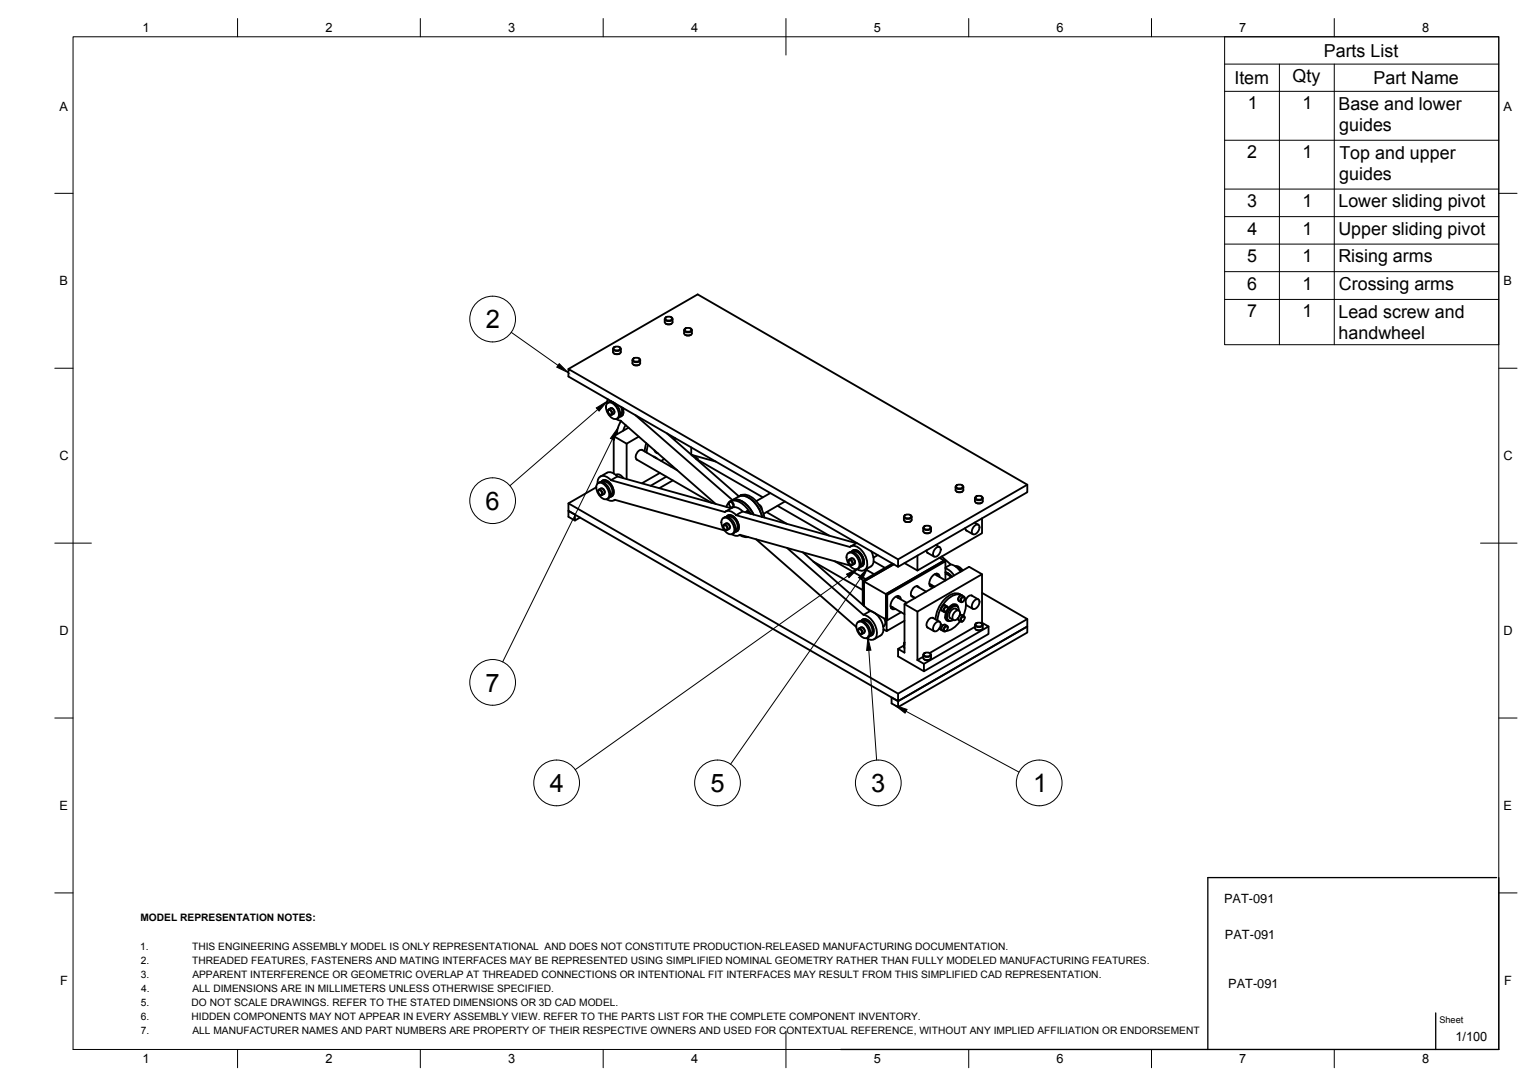
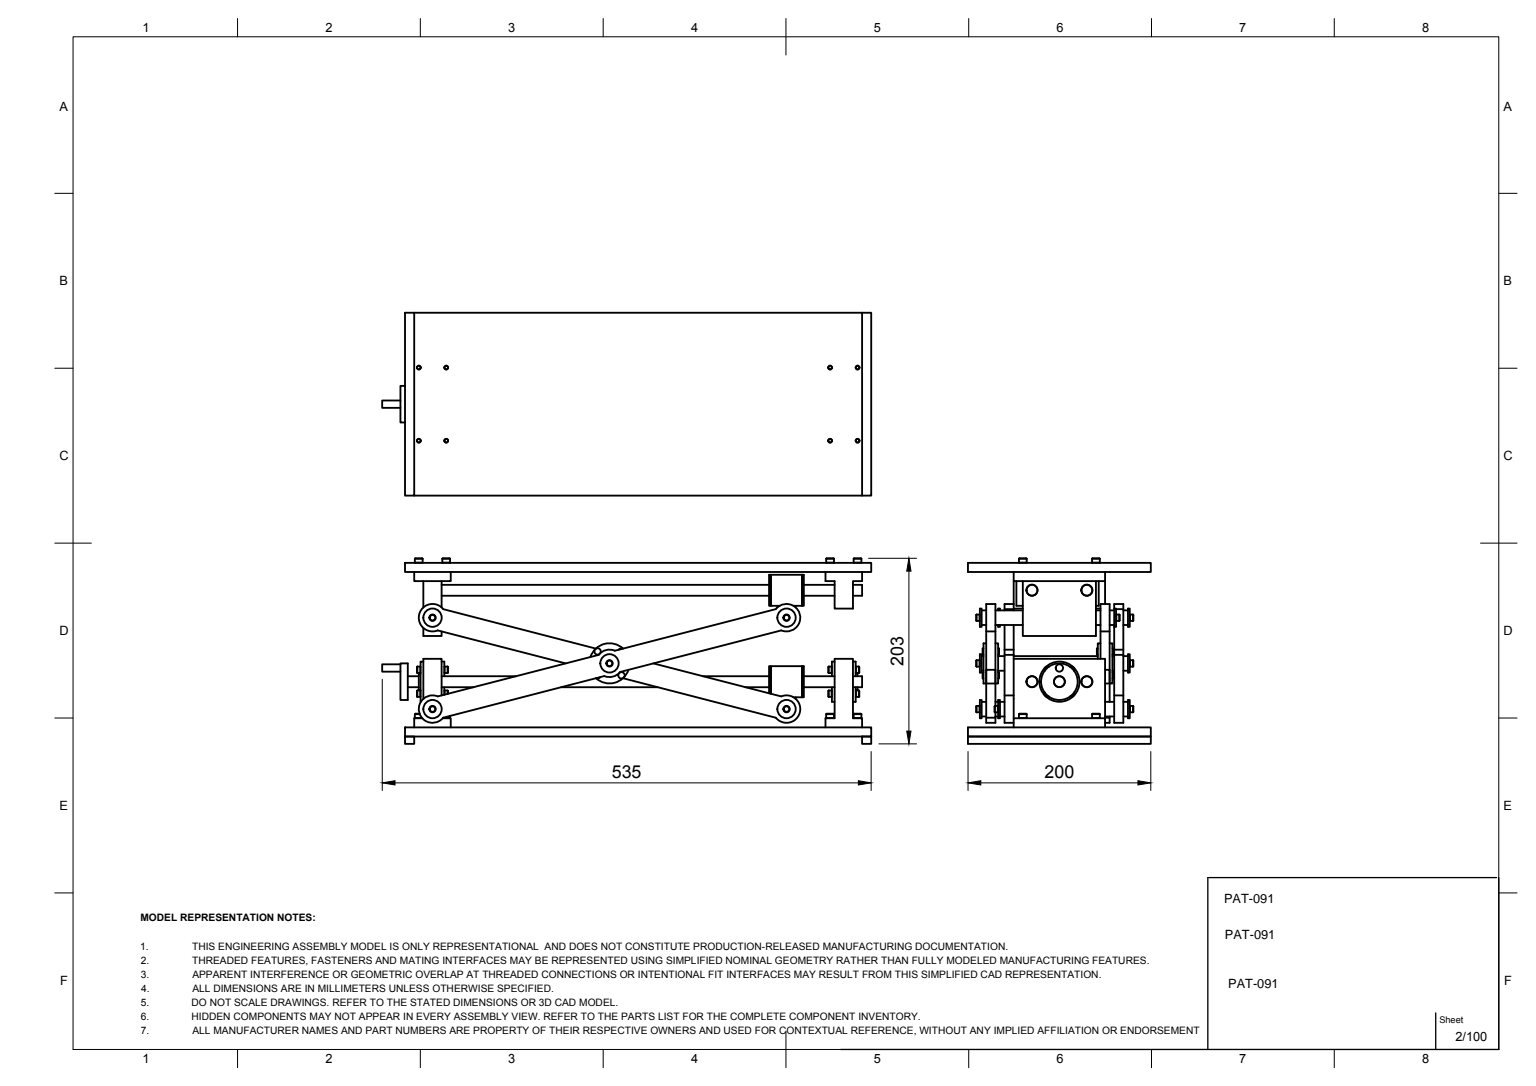
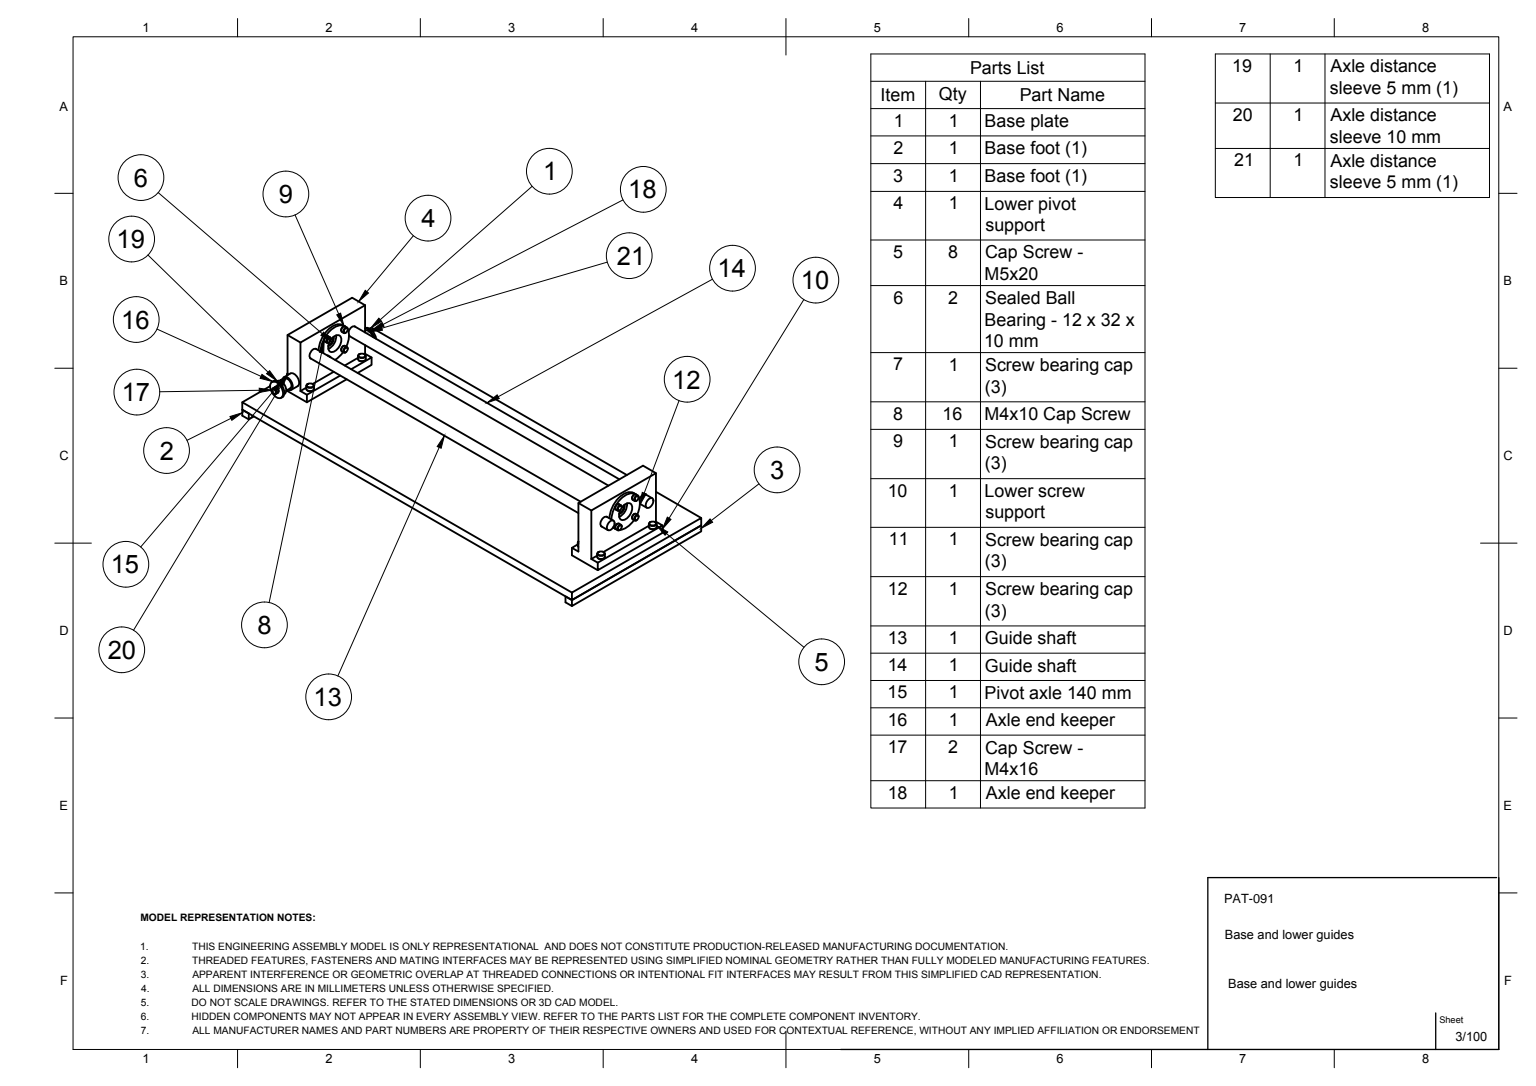
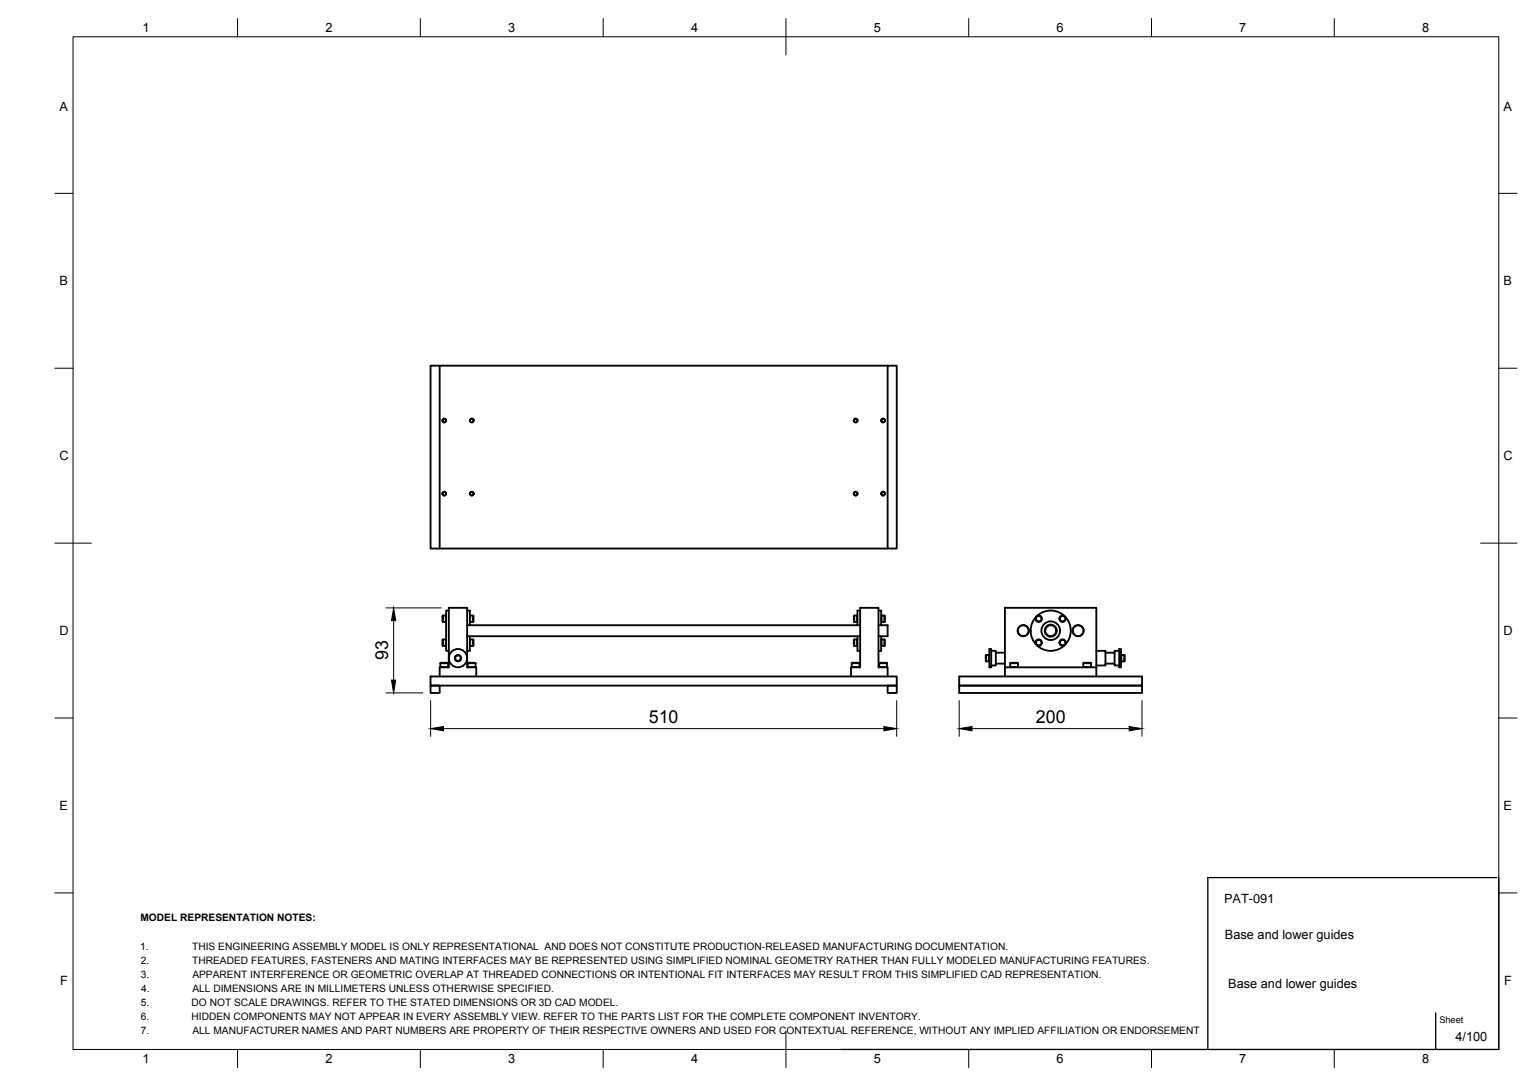
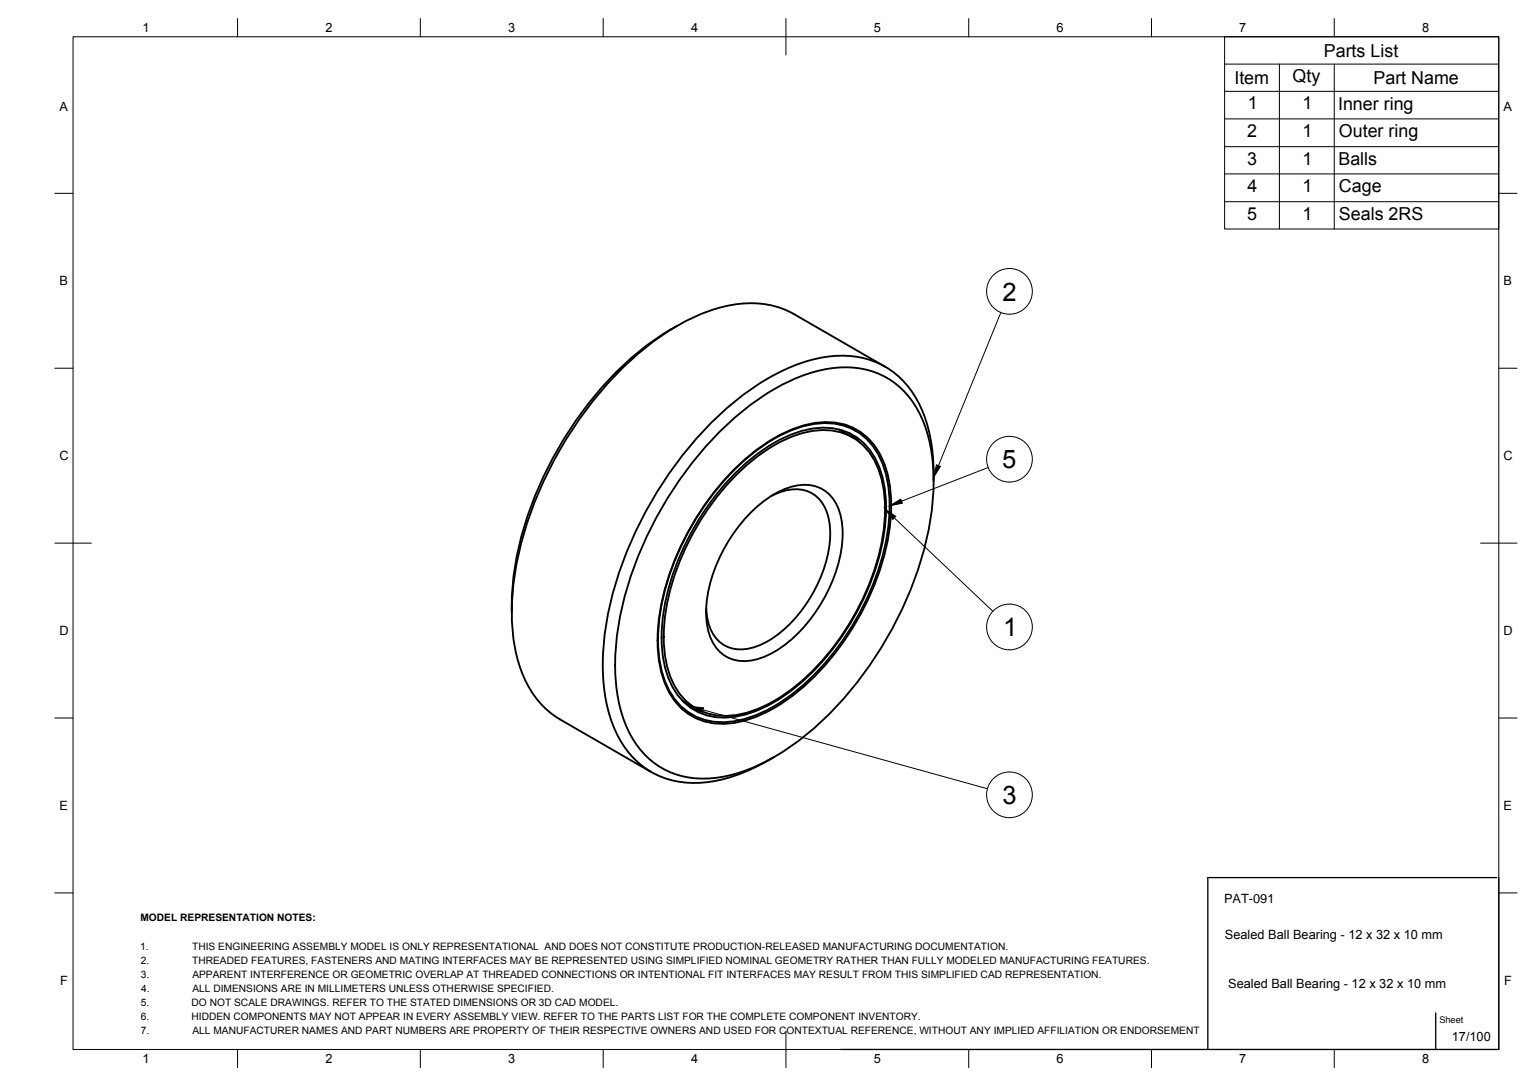
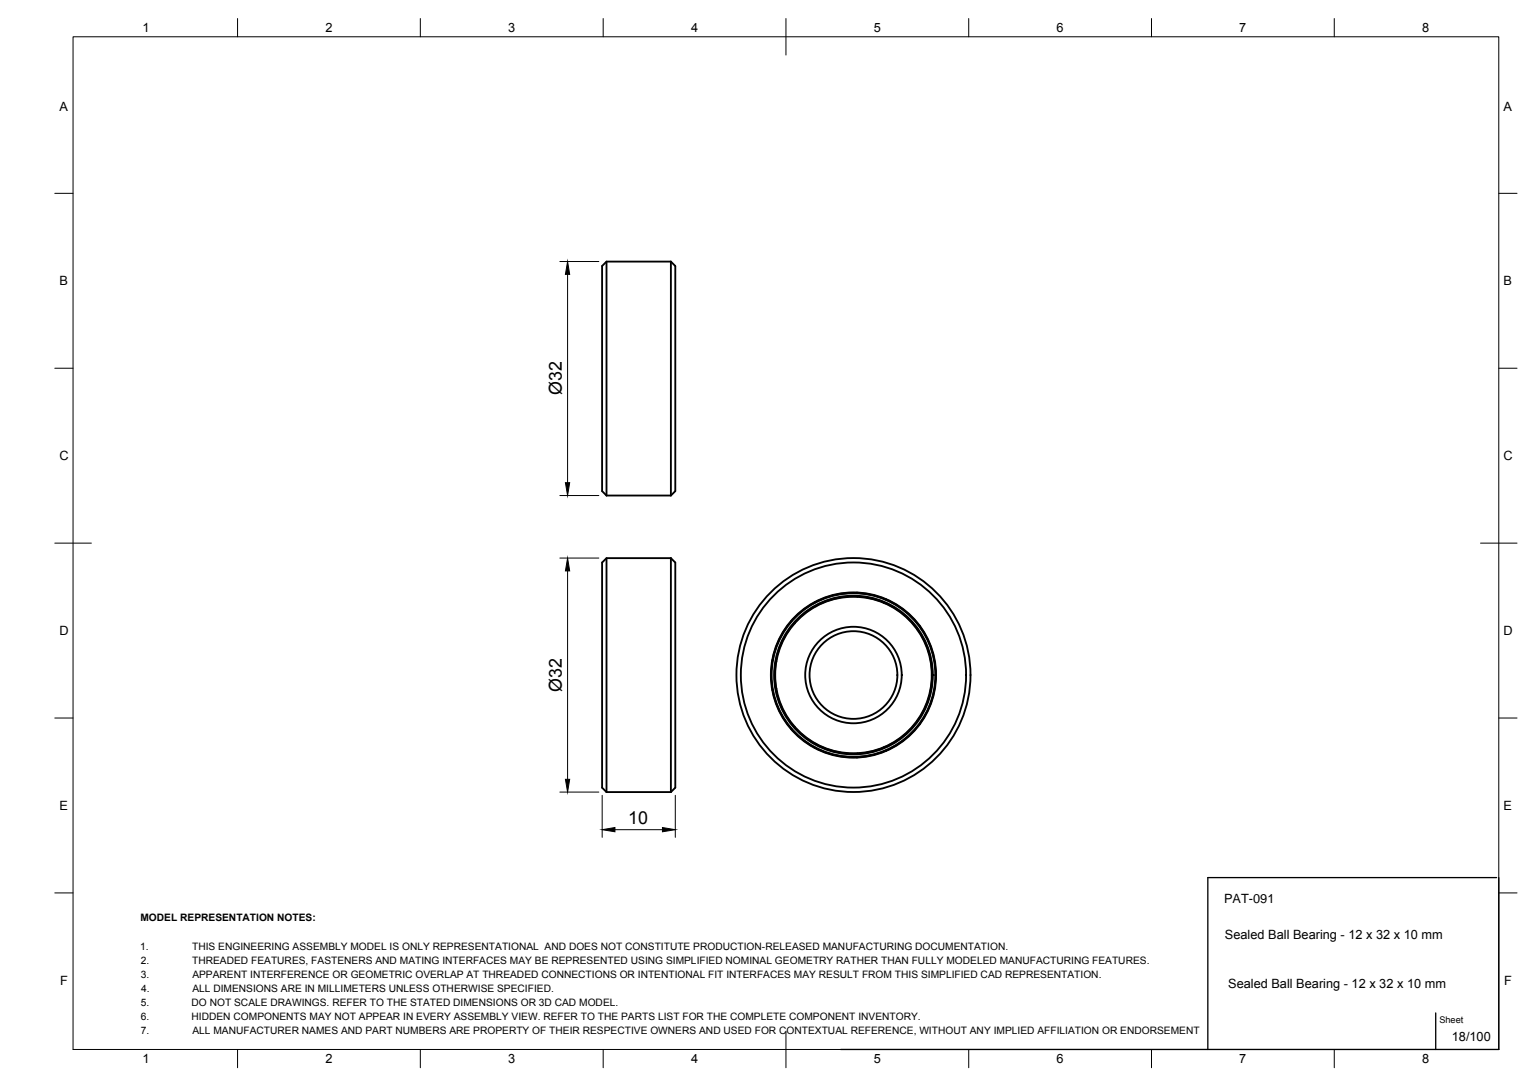
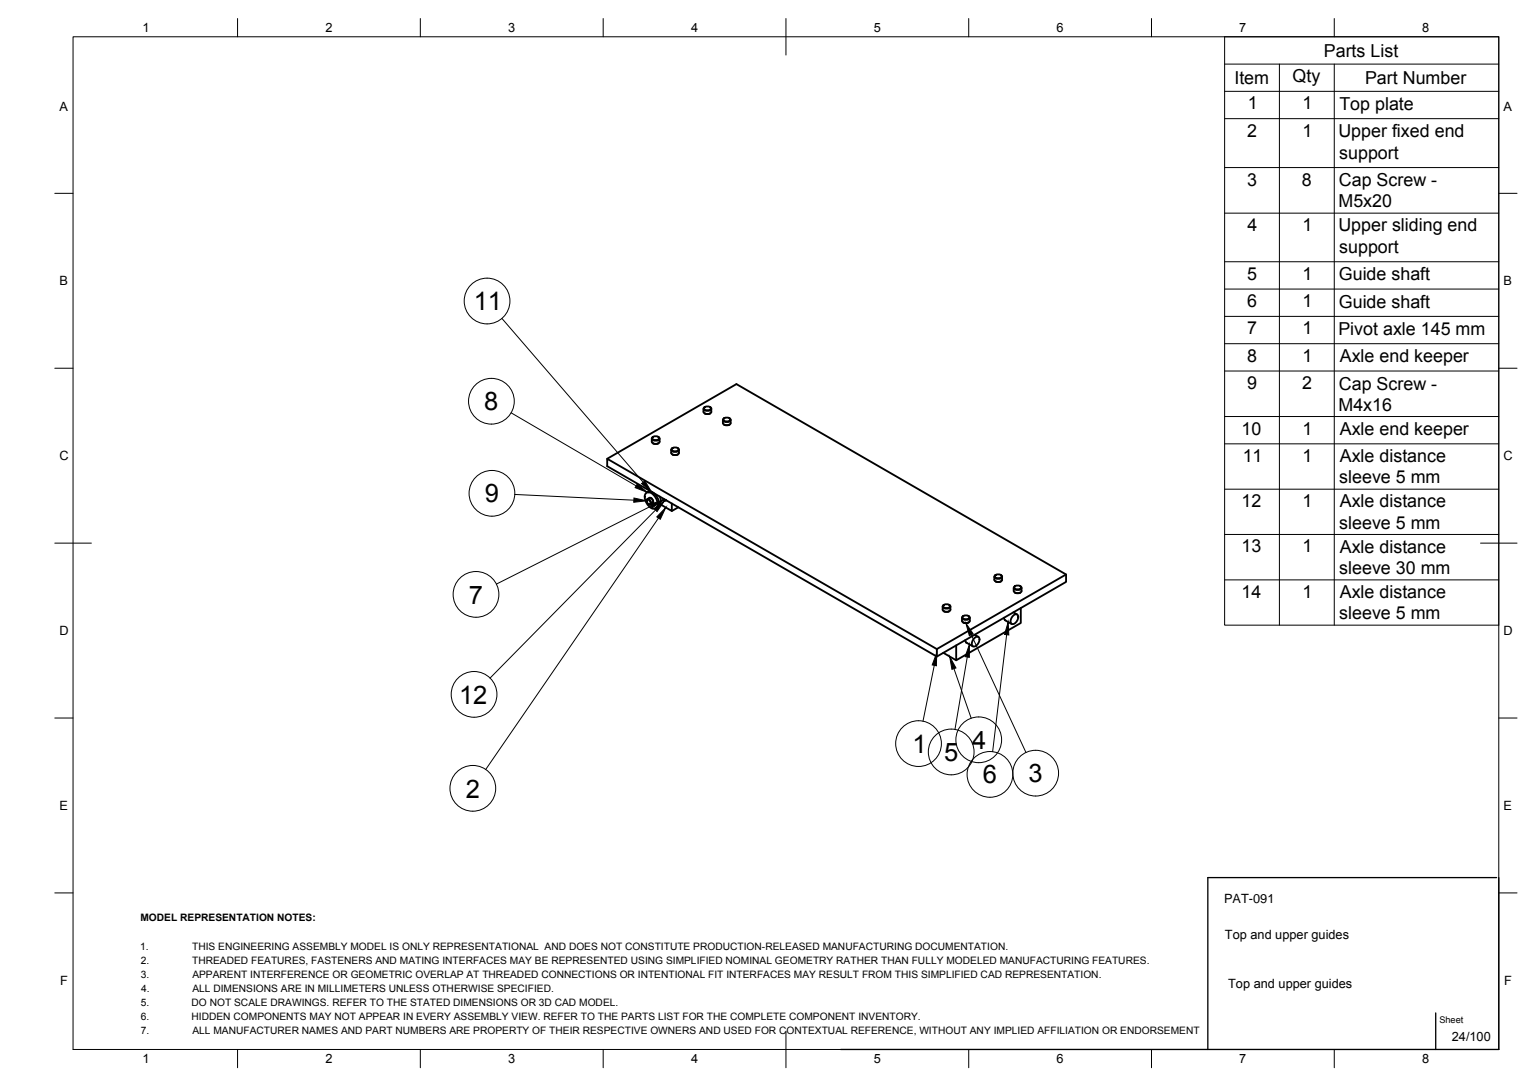
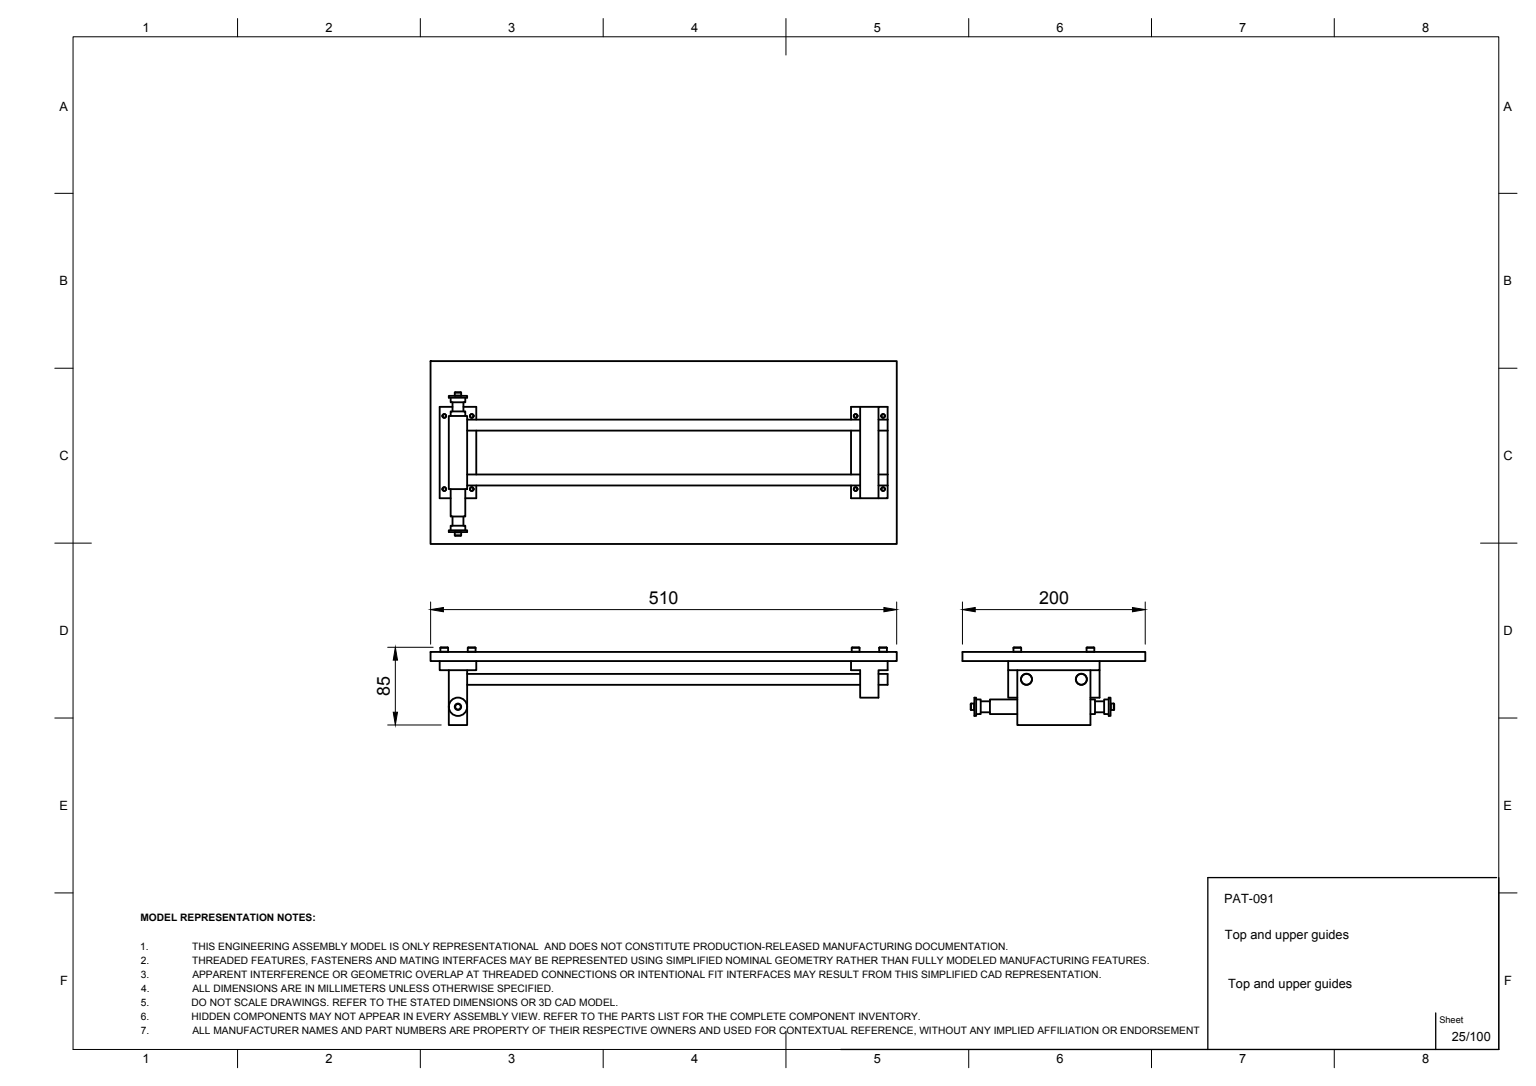
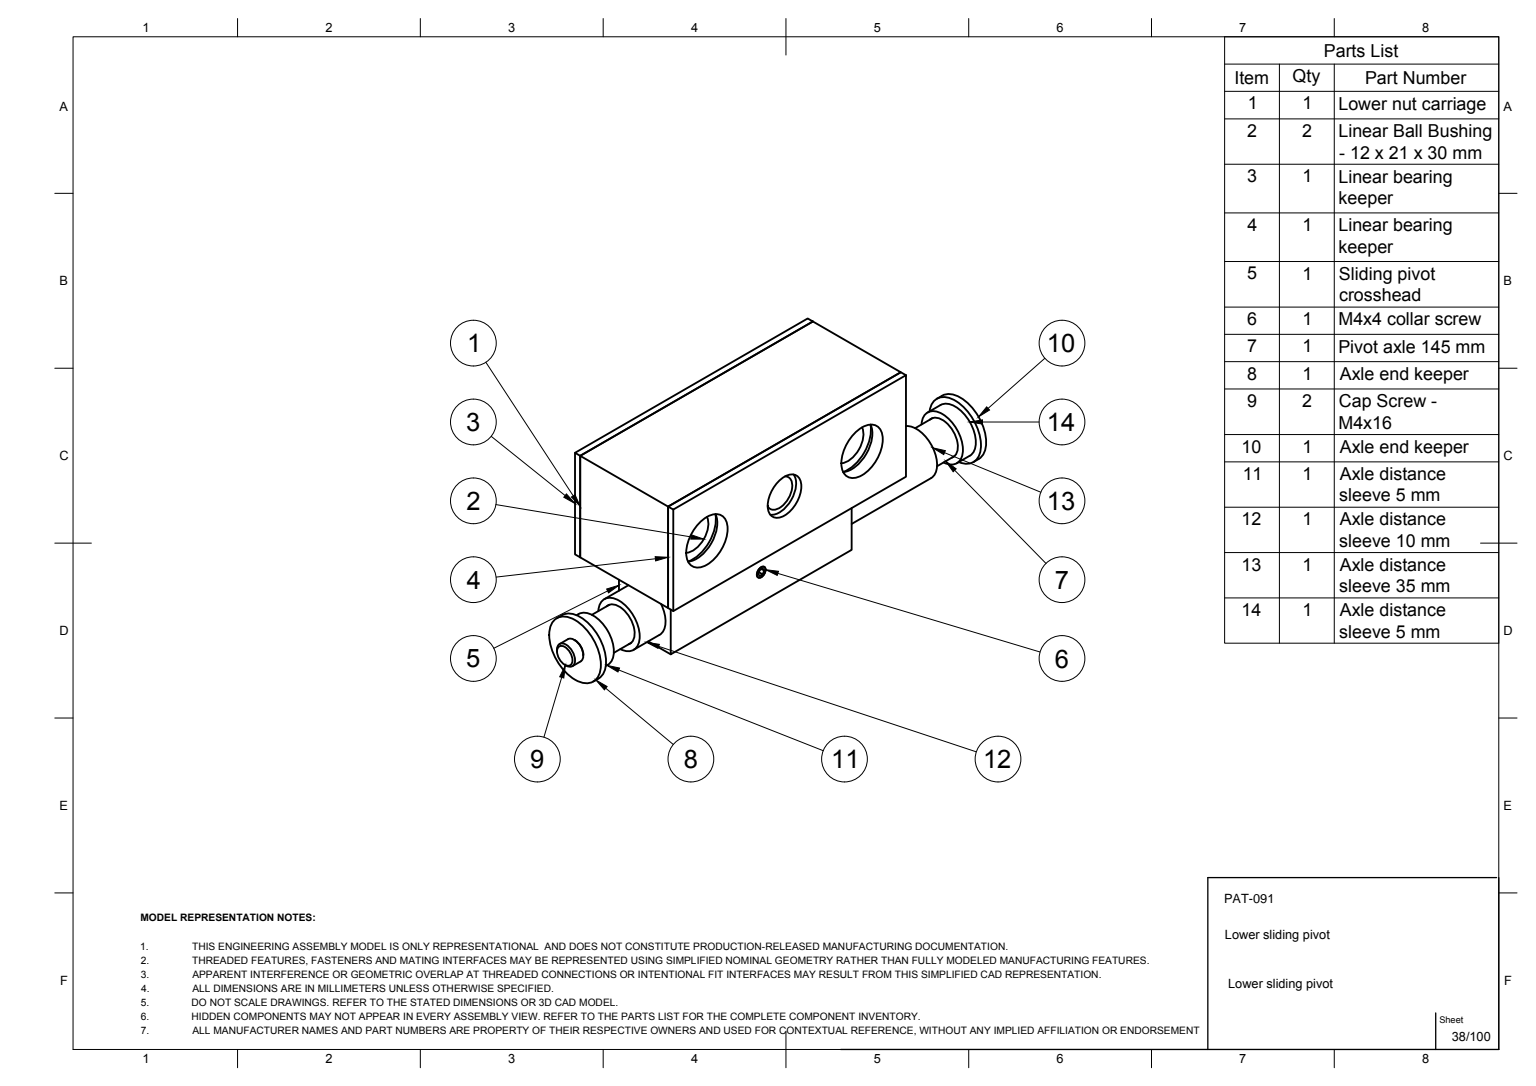
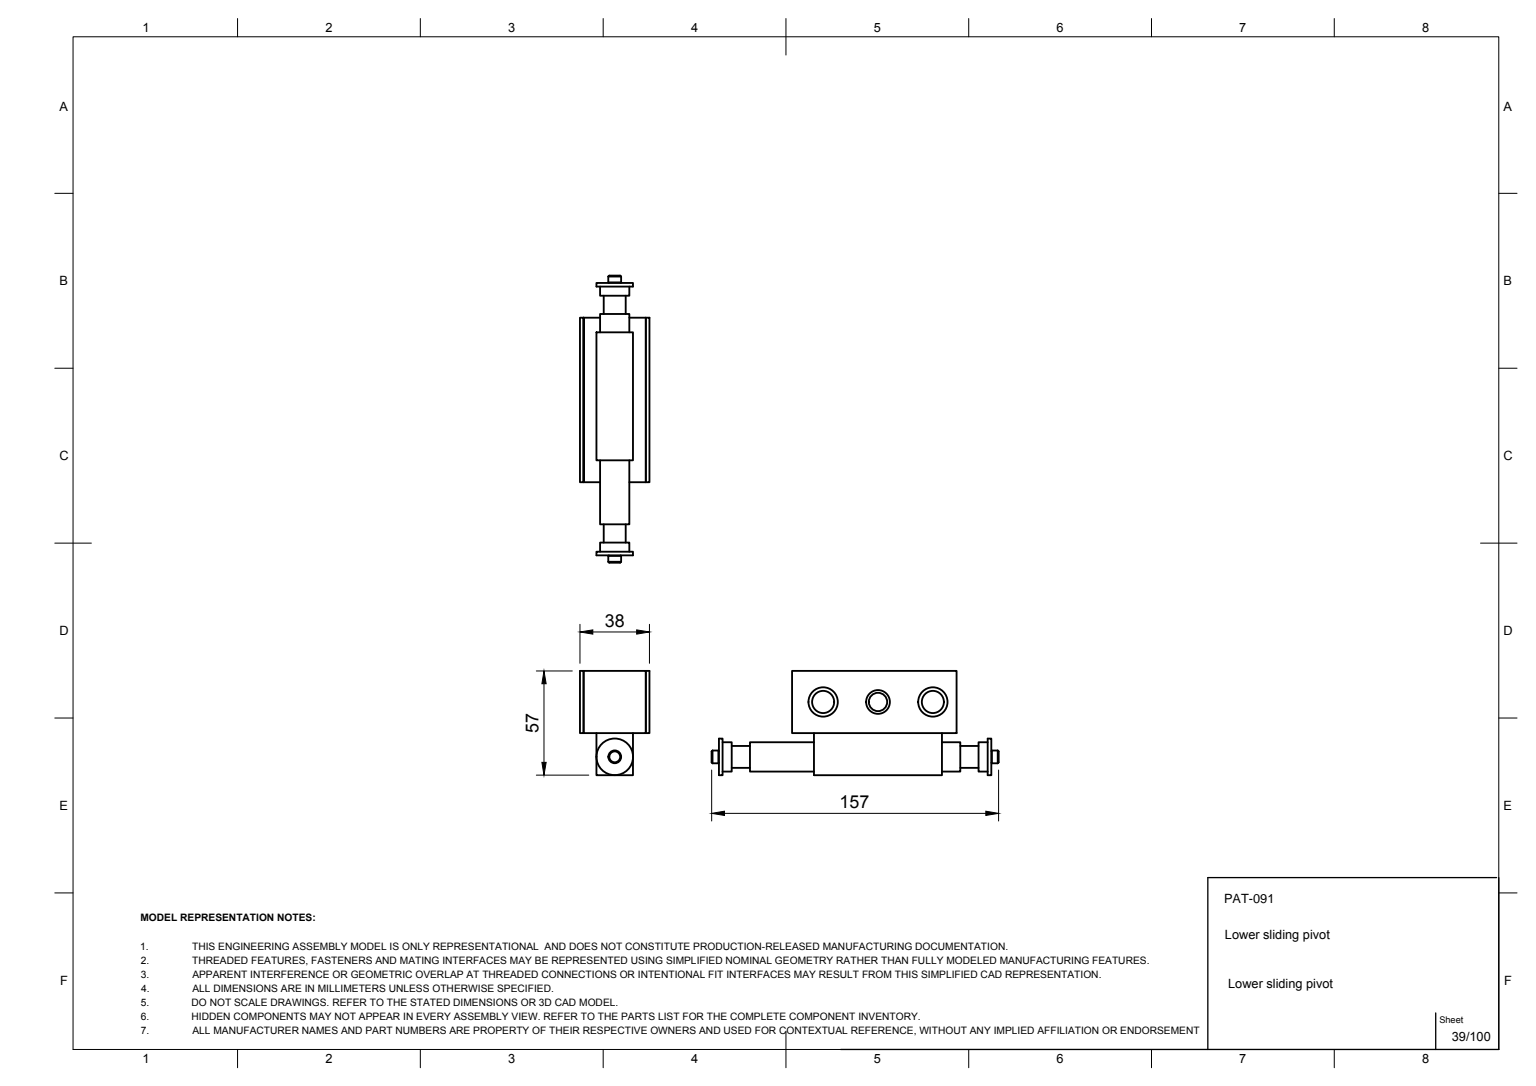
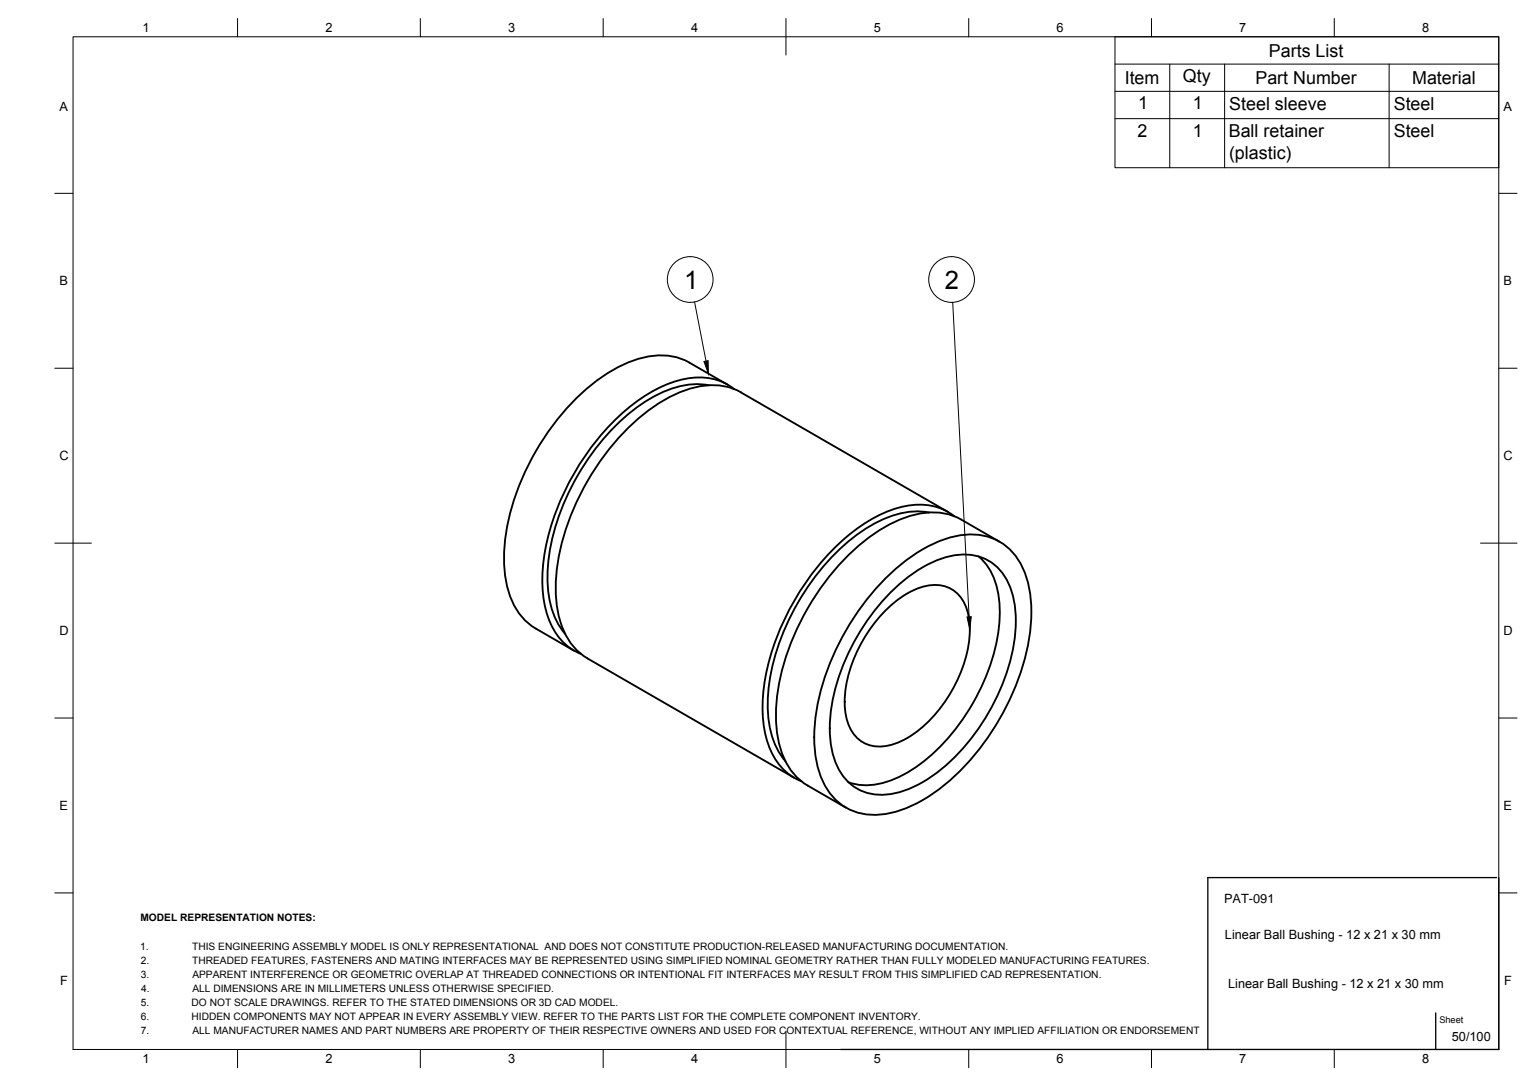
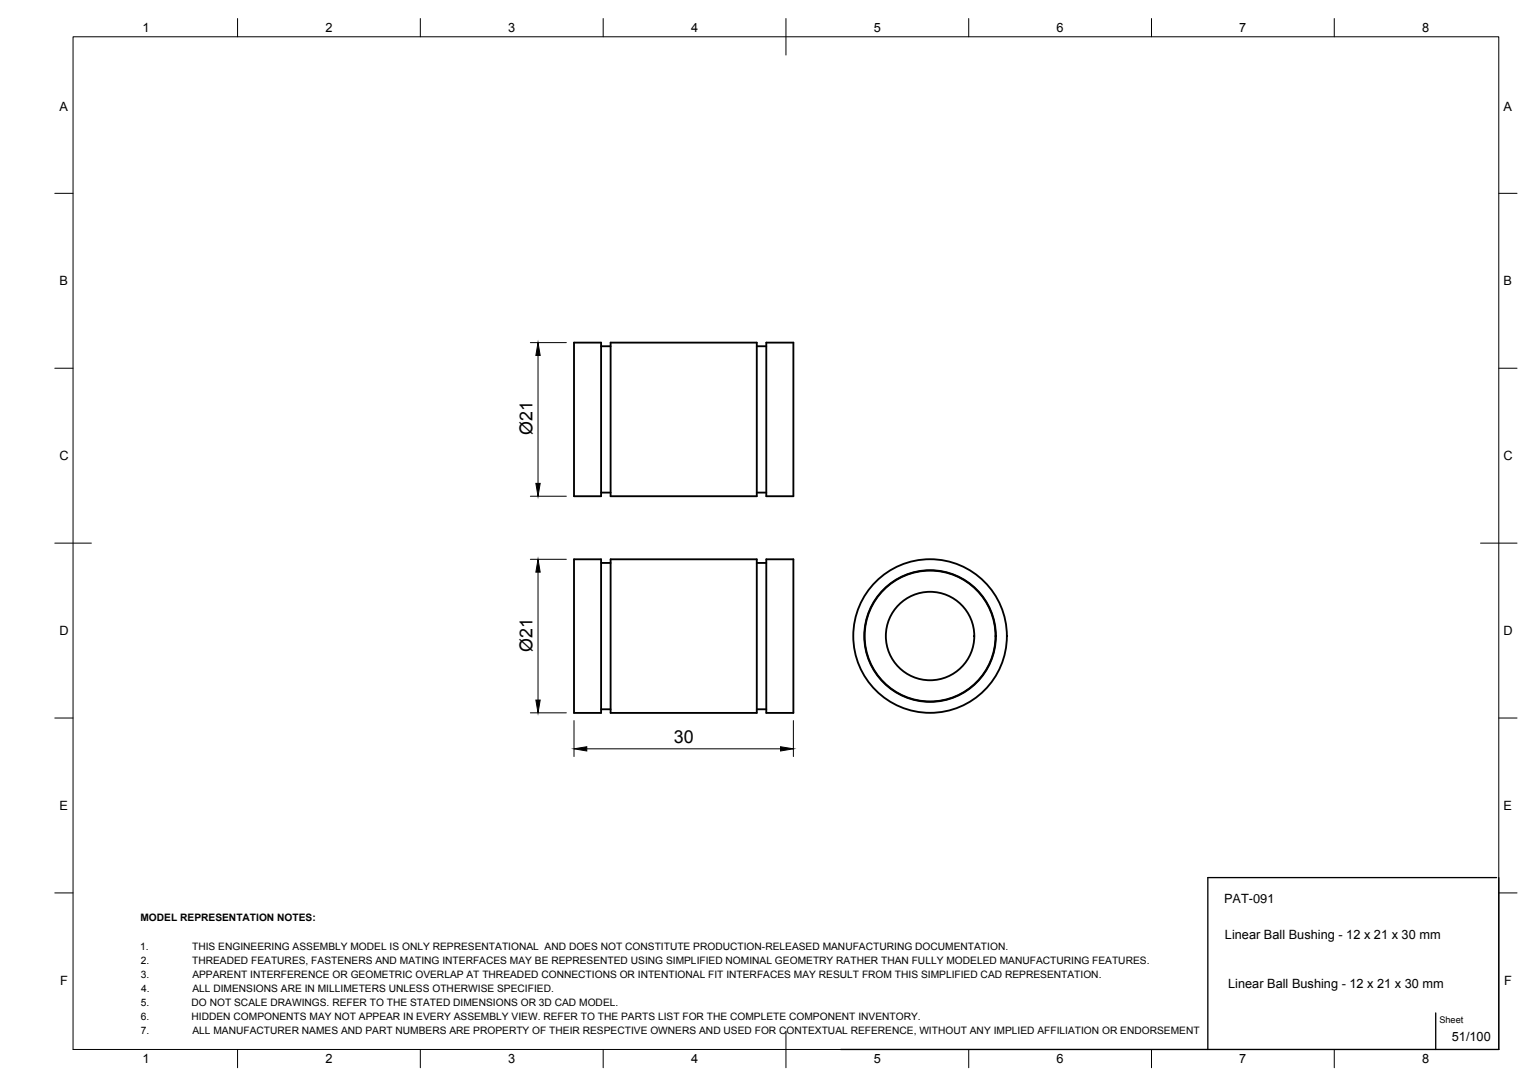
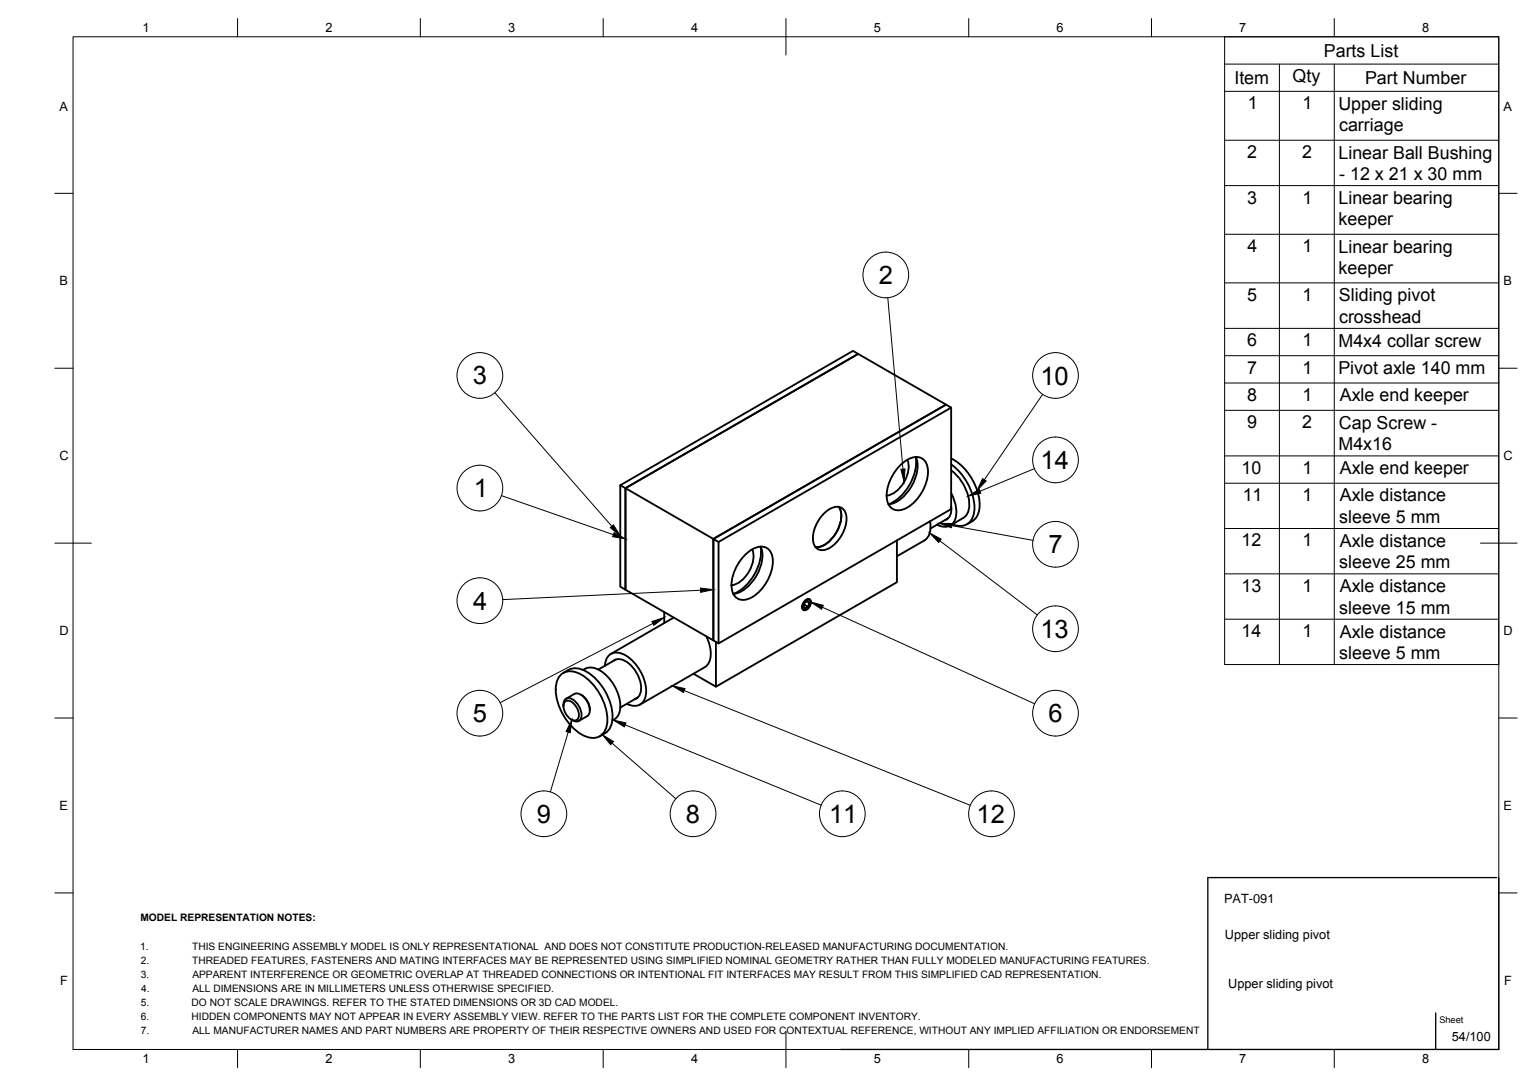
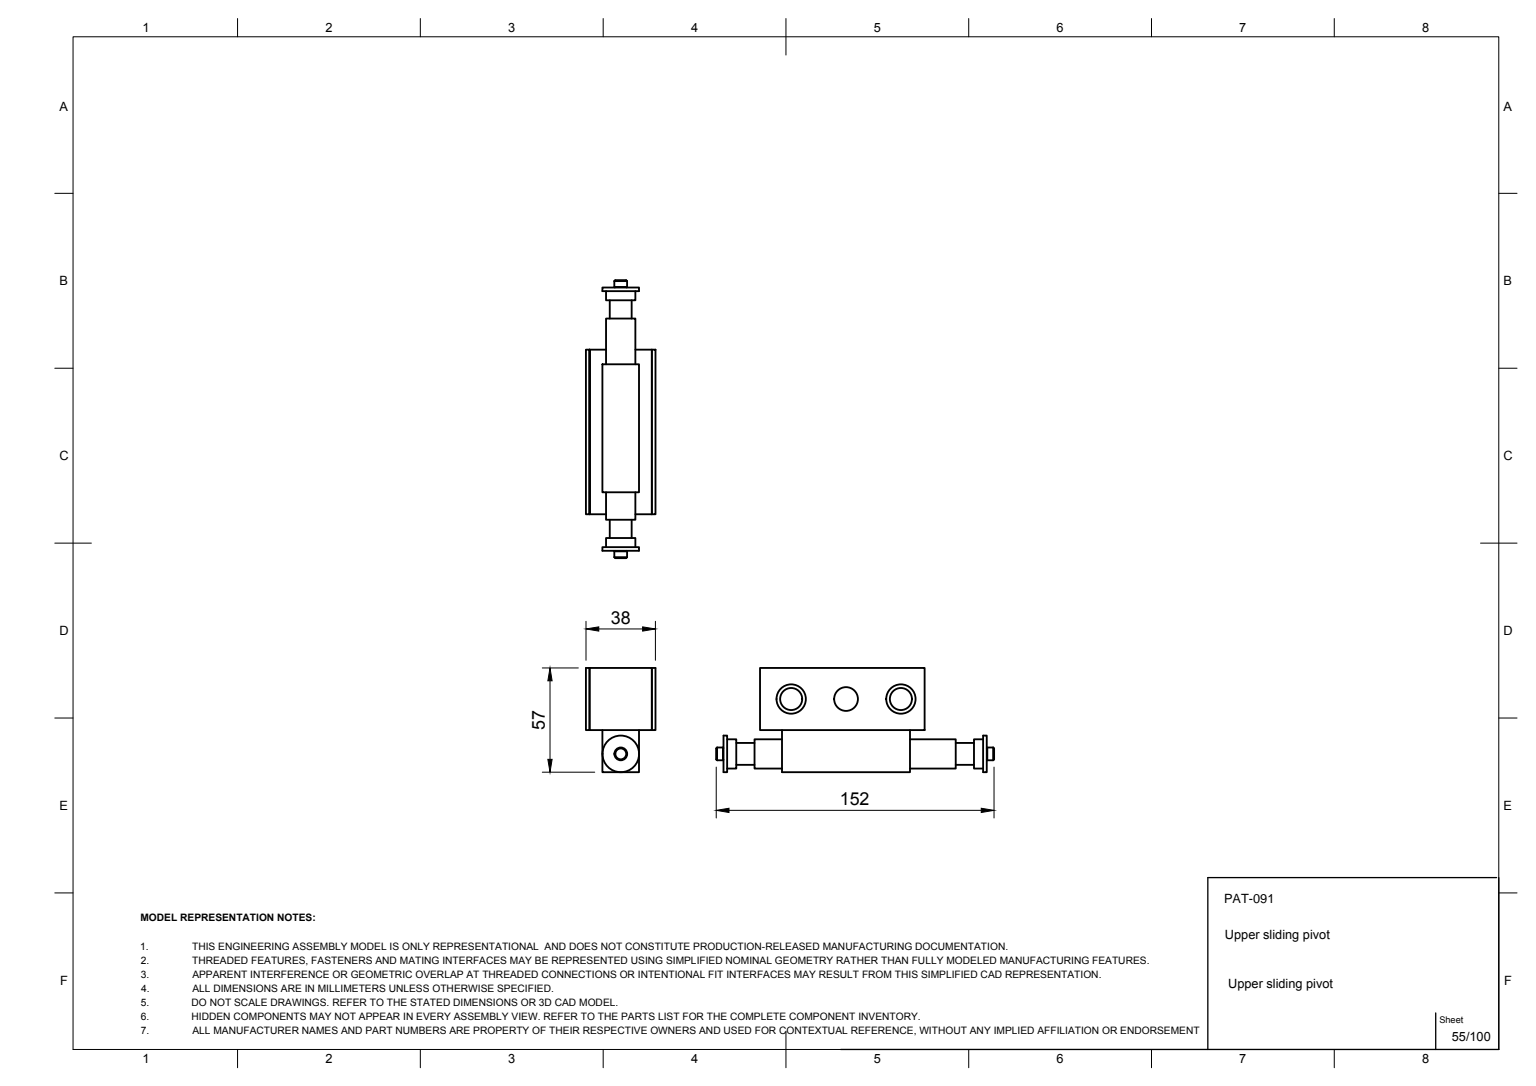
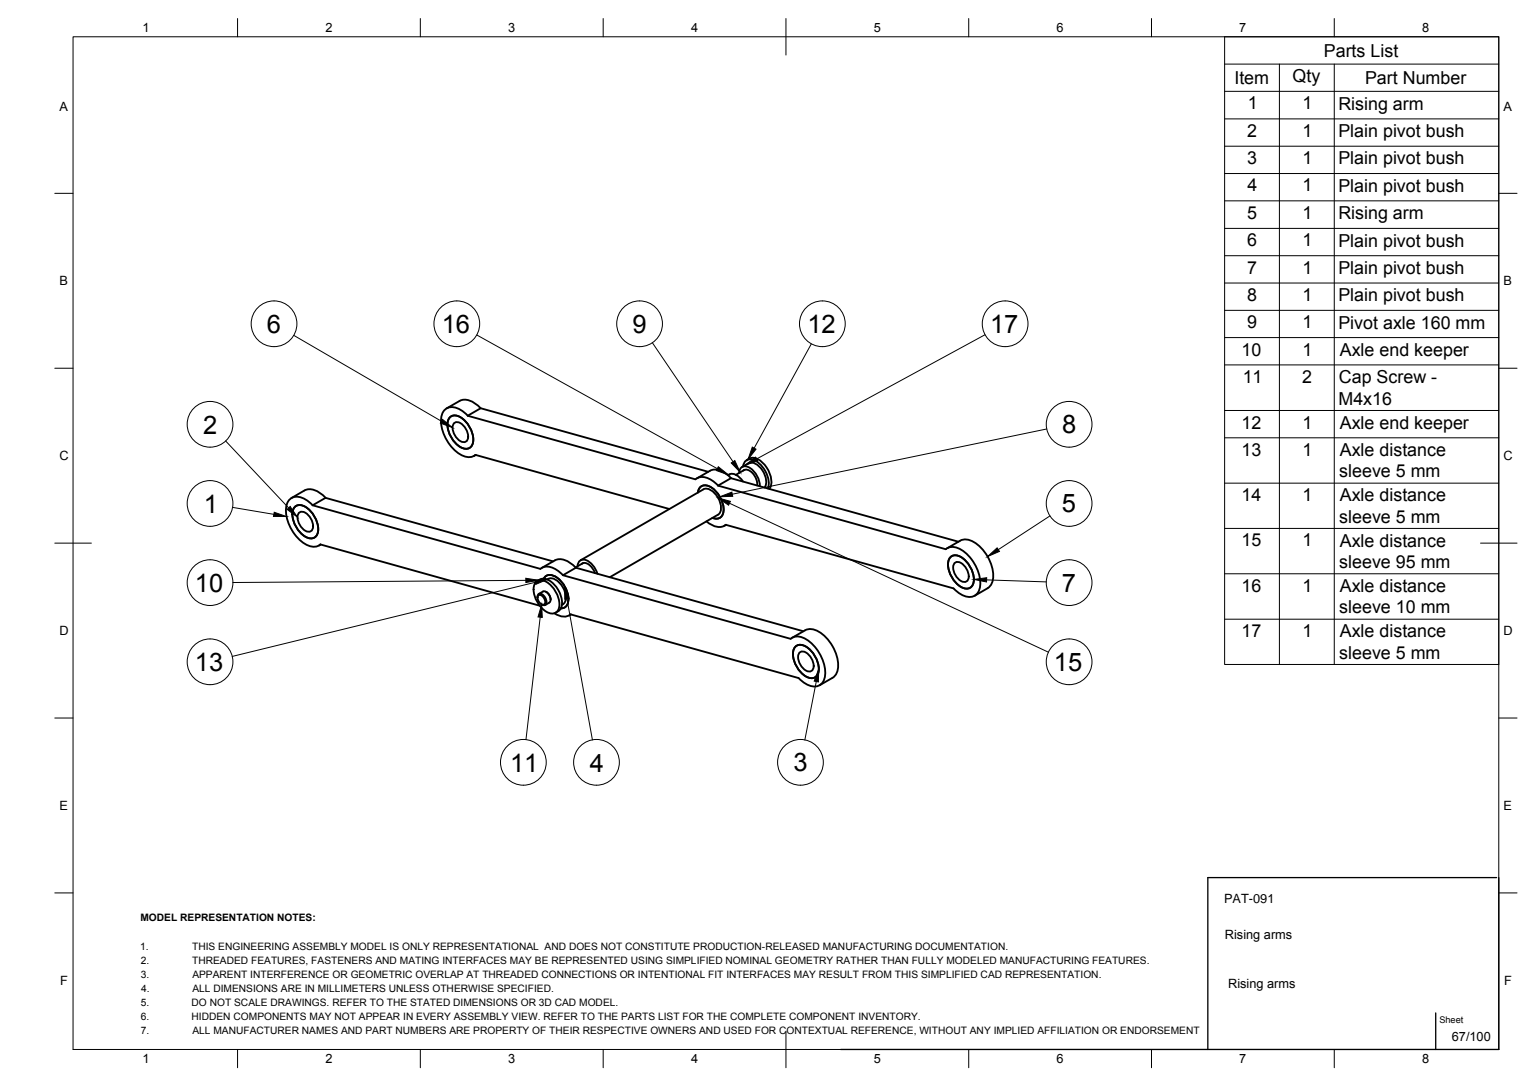
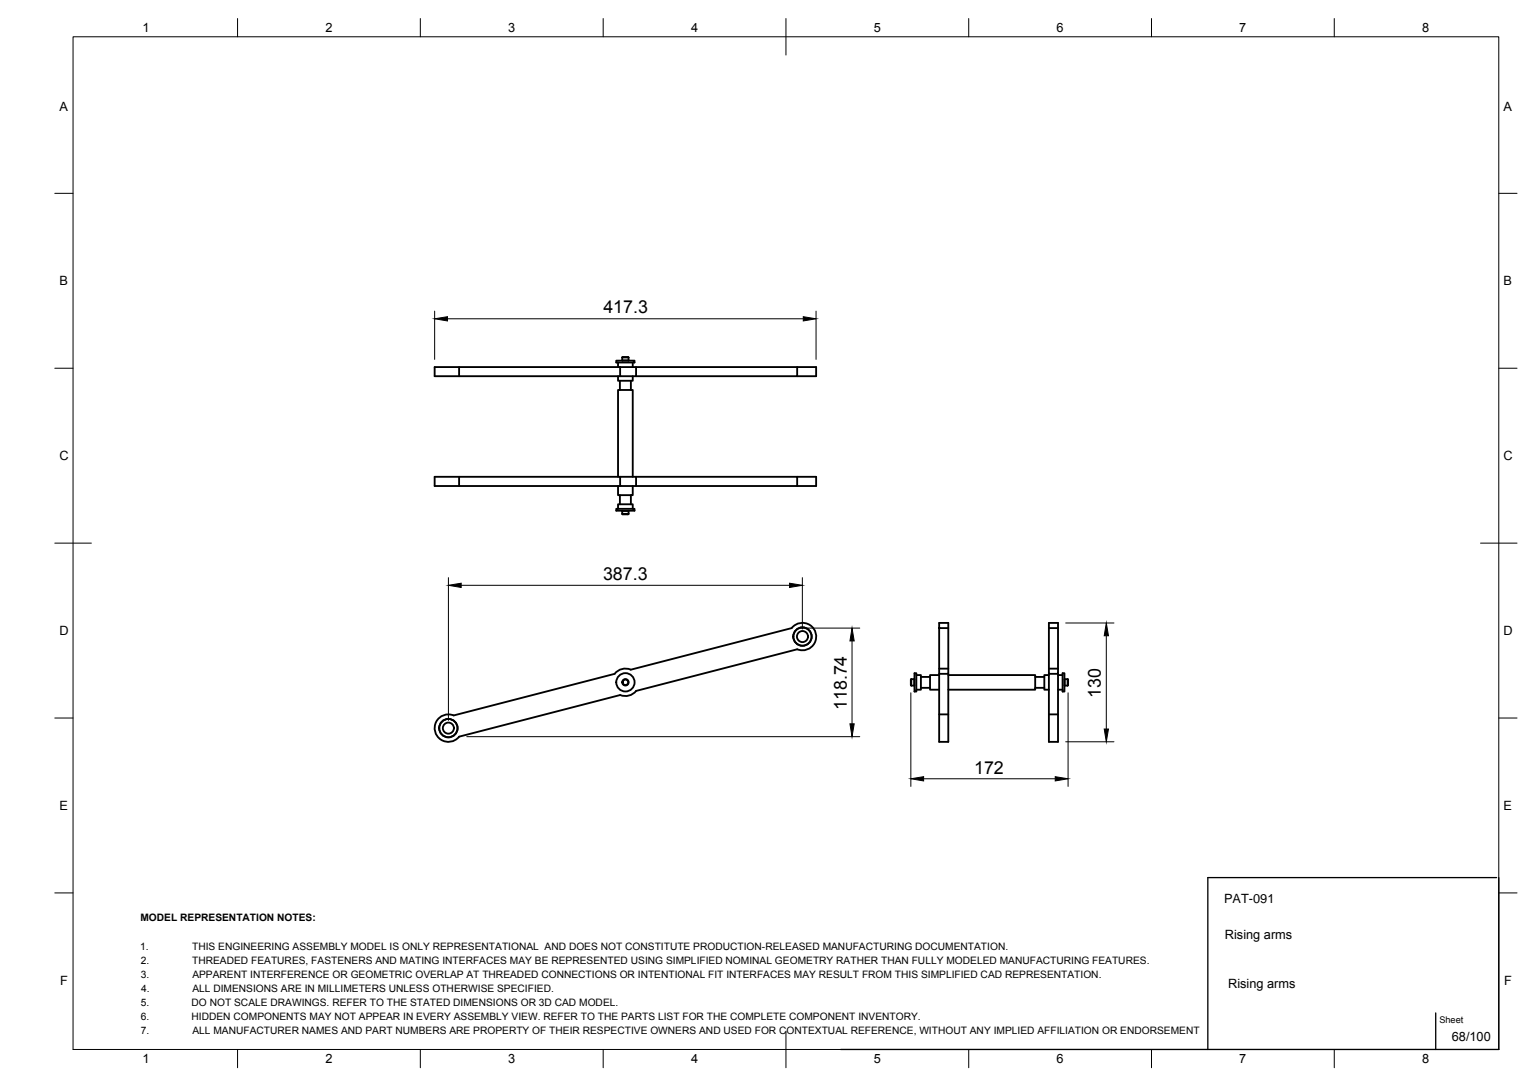
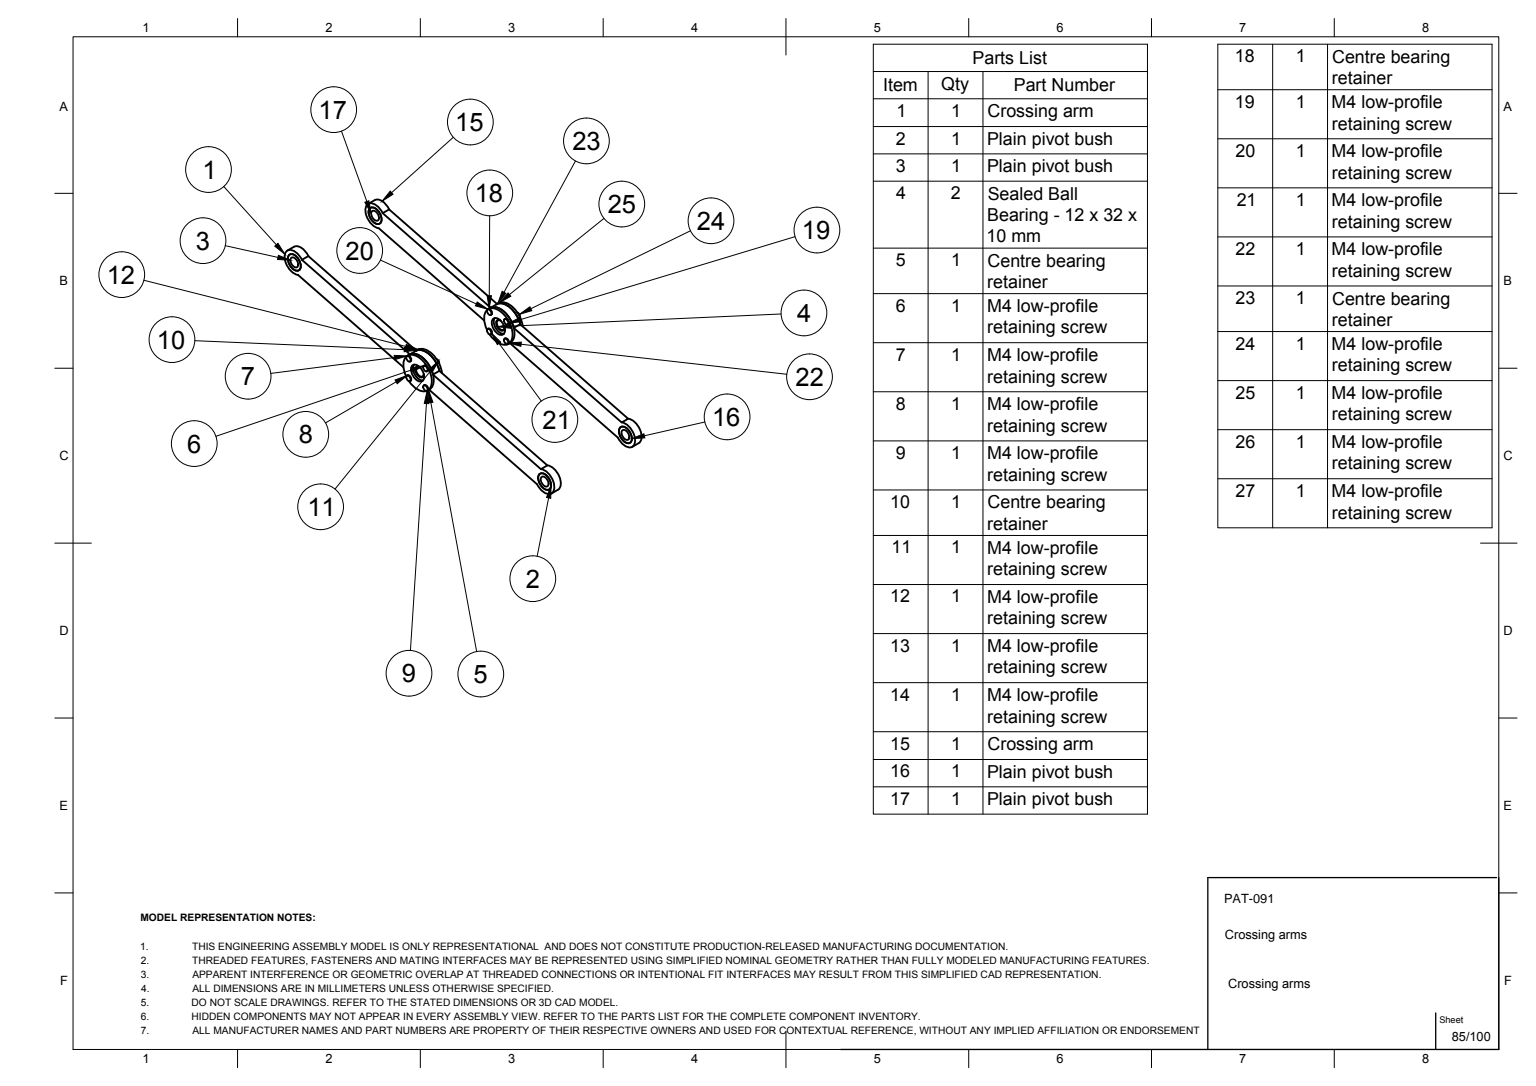
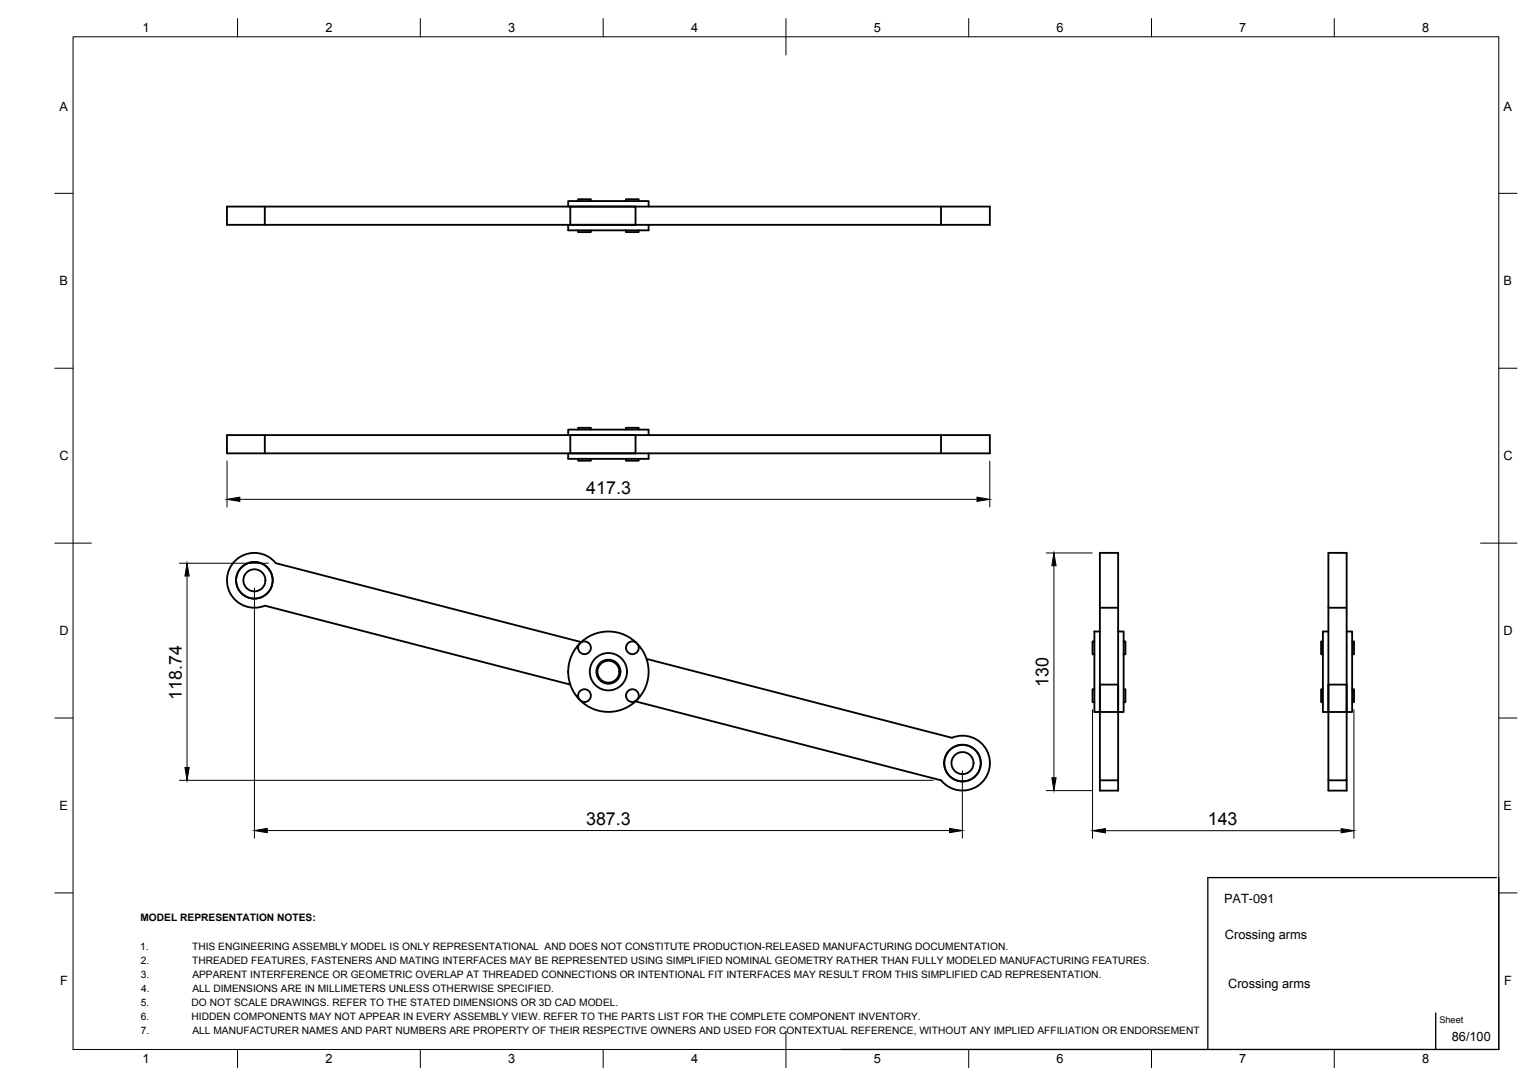
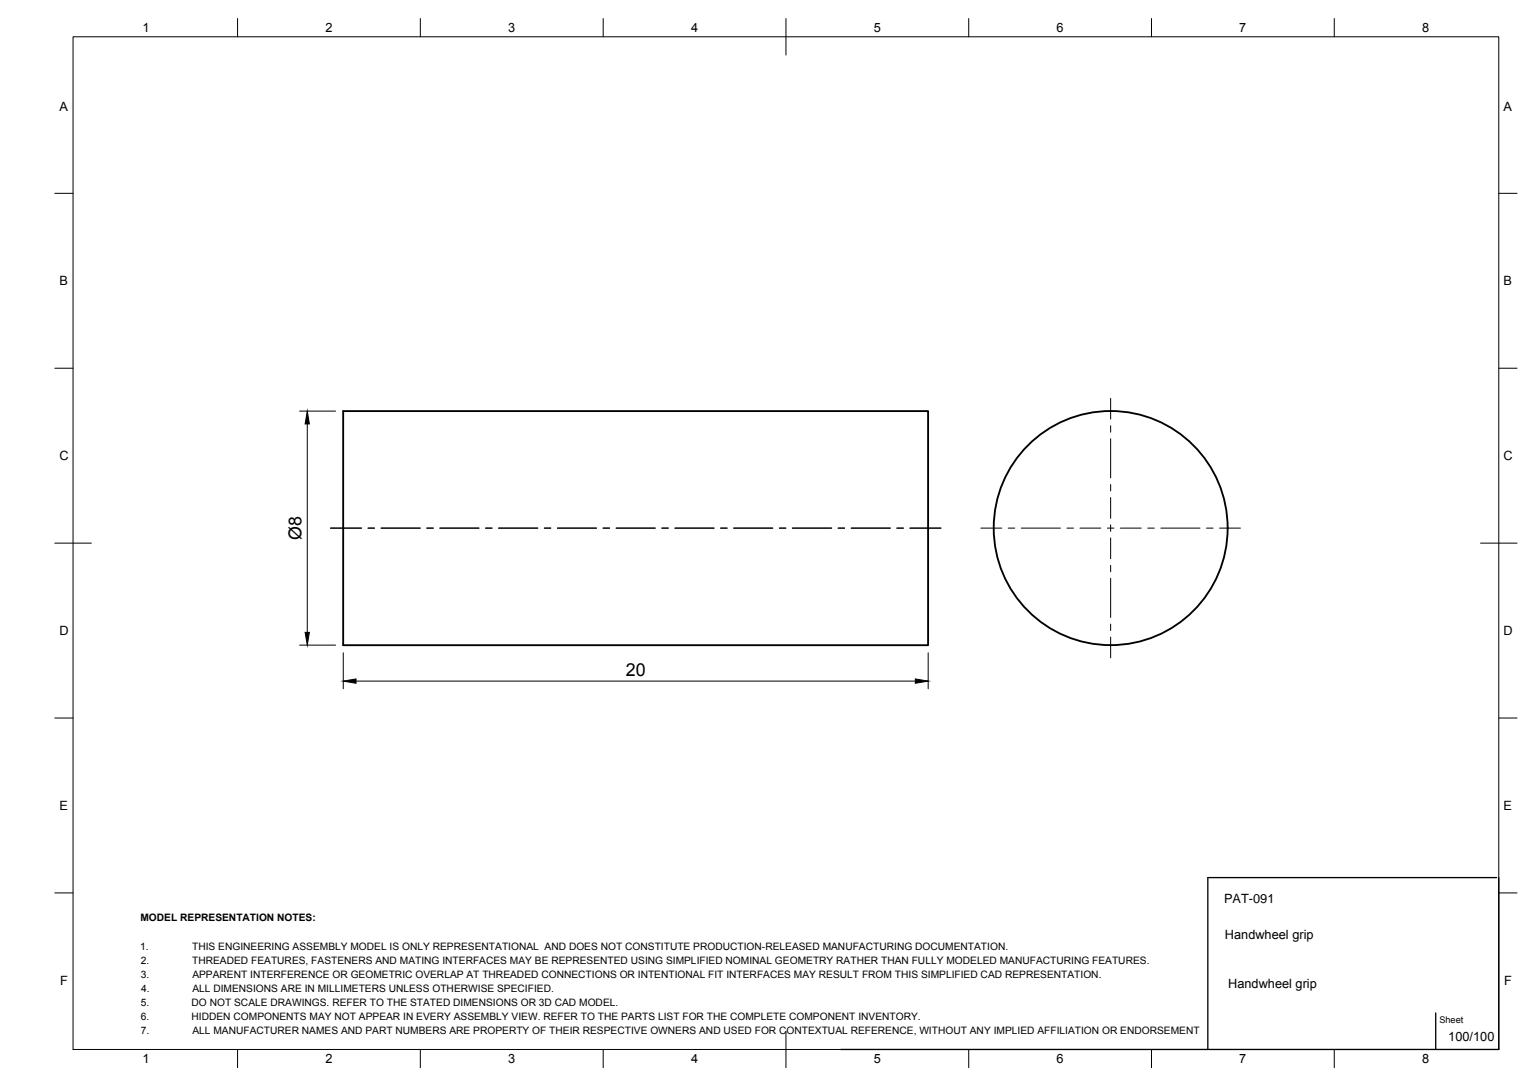
ISO-10303-21;
HEADER;
/* Generated by software containing ST-Developer
 * from STEP Tools, Inc. (www.steptools.com) 
 */

FILE_DESCRIPTION(
/* description */ ('PAT-091'),
/* implementation_level */ '2;1');

FILE_NAME(
/* name */ 'PAT-091',
/* time_stamp */ '2026-10-27T15:34:44-07:00',
/* author */ (''),
/* organization */ (''),
/* preprocessor_version */ 'ST-DEVELOPER v20.2',
/* originating_system */ 'Autodesk Translation Framework v15.17.0.0',
/* authorisation */ '');

FILE_SCHEMA (('AUTOMOTIVE_DESIGN { 1 0 10303 214 3 1 1 }'));
ENDSEC;

DATA;
#10=MECHANICAL_DESIGN_GEOMETRIC_PRESENTATION_REPRESENTATION('',(#971,#972,
#973,#974,#975,#976,#977,#978,#979,#980,#981,#982,#983,#984,#985,#986,#987,
#988,#989,#990,#991,#992,#993,#994,#995,#996,#997,#998,#999,#1000,#1001,
#1002,#1003,#1004,#1005,#1006,#1007,#1008,#1009,#1010,#1011,#1012,#1013,
#1014,#1015,#1016,#1017,#1018,#1019,#1020,#1021,#1022,#1023,#1024,#1025,
#1026,#1027,#1028,#1029,#1030,#1031,#1032,#1033,#1034,#1035,#1036,#1037,
#1038,#1039,#1040,#1041,#1042,#1043,#1044,#1045,#1046,#1047,#1048,#1049,
#1050,#1051,#1052,#1053,#1054,#1055,#1056,#1057,#1058,#1059,#1060,#1061,
#1062,#1063,#1064,#1065,#1066,#1067,#1068,#1069,#1070,#1071,#1072,#1073,
#1074,#1075,#1076,#1077,#1078,#1079,#1080,#1081,#1082,#1083,#1084,#1085,
#1086,#1087,#1088,#1089,#1090,#1091,#1092,#1093,#1094),#25100);
#11=CONTEXT_DEPENDENT_OVER_RIDING_STYLED_ITEM('',(#26115),#25531,#1094,
(#361,#204));
#12=MAPPED_ITEM('',#13,#16467);
#13=REPRESENTATION_MAP(#16467,#25510);
#14=SPHERICAL_SURFACE('',#16174,0.29765);
#15=SPHERICAL_SURFACE('',#16176,0.29765);
#16=SPHERICAL_SURFACE('',#16178,0.29765);
#17=SPHERICAL_SURFACE('',#16180,0.29765);
#18=SPHERICAL_SURFACE('',#16182,0.29765);
#19=SPHERICAL_SURFACE('',#16184,0.29765);
#20=SPHERICAL_SURFACE('',#16186,0.29765);
#21=SPHERICAL_SURFACE('',#16189,0.321462);
#22=SPHERICAL_SURFACE('',#16202,0.321462);
#23=SPHERICAL_SURFACE('',#16203,0.321462);
#24=SPHERICAL_SURFACE('',#16216,0.321462);
#25=SPHERICAL_SURFACE('',#16217,0.321462);
#26=SPHERICAL_SURFACE('',#16230,0.321462);
#27=SPHERICAL_SURFACE('',#16231,0.321462);
#28=SPHERICAL_SURFACE('',#16244,0.321462);
#29=SPHERICAL_SURFACE('',#16245,0.321462);
#30=SPHERICAL_SURFACE('',#16258,0.321462);
#31=SPHERICAL_SURFACE('',#16259,0.321462);
#32=SPHERICAL_SURFACE('',#16272,0.321462);
#33=SPHERICAL_SURFACE('',#16280,0.321462);
#34=SPHERICAL_SURFACE('',#16286,0.321462);
#35=TOROIDAL_SURFACE('',#16134,1.1,0.309556);
#36=TOROIDAL_SURFACE('',#16154,1.1,0.309556);
#37=ITEM_DEFINED_TRANSFORMATION($,$,#15419,#15468);
#38=ITEM_DEFINED_TRANSFORMATION($,$,#15451,#15469);
#39=ITEM_DEFINED_TRANSFORMATION($,$,#14919,#15699);
#40=ITEM_DEFINED_TRANSFORMATION($,$,#14950,#15700);
#41=ITEM_DEFINED_TRANSFORMATION($,$,#14983,#15701);
#42=ITEM_DEFINED_TRANSFORMATION($,$,#15012,#15702);
#43=ITEM_DEFINED_TRANSFORMATION($,$,#15018,#15703);
#44=ITEM_DEFINED_TRANSFORMATION($,$,#15024,#15704);
#45=ITEM_DEFINED_TRANSFORMATION($,$,#15038,#15705);
#46=ITEM_DEFINED_TRANSFORMATION($,$,#15047,#15706);
#47=ITEM_DEFINED_TRANSFORMATION($,$,#15056,#15707);
#48=ITEM_DEFINED_TRANSFORMATION($,$,#15065,#15708);
#49=ITEM_DEFINED_TRANSFORMATION($,$,#15074,#15709);
#50=ITEM_DEFINED_TRANSFORMATION($,$,#15083,#15710);
#51=ITEM_DEFINED_TRANSFORMATION($,$,#15092,#15711);
#52=ITEM_DEFINED_TRANSFORMATION($,$,#15092,#15712);
#53=ITEM_DEFINED_TRANSFORMATION($,$,#15092,#15713);
#54=ITEM_DEFINED_TRANSFORMATION($,$,#15092,#15714);
#55=ITEM_DEFINED_TRANSFORMATION($,$,#15092,#15715);
#56=ITEM_DEFINED_TRANSFORMATION($,$,#15092,#15716);
#57=ITEM_DEFINED_TRANSFORMATION($,$,#15092,#15717);
#58=ITEM_DEFINED_TRANSFORMATION($,$,#15092,#15718);
#59=ITEM_DEFINED_TRANSFORMATION($,$,#15673,#15719);
#60=ITEM_DEFINED_TRANSFORMATION($,$,#15673,#15720);
#61=ITEM_DEFINED_TRANSFORMATION($,$,#15119,#15721);
#62=ITEM_DEFINED_TRANSFORMATION($,$,#15135,#15722);
#63=ITEM_DEFINED_TRANSFORMATION($,$,#15159,#15723);
#64=ITEM_DEFINED_TRANSFORMATION($,$,#15183,#15724);
#65=ITEM_DEFINED_TRANSFORMATION($,$,#15200,#15725);
#66=ITEM_DEFINED_TRANSFORMATION($,$,#15214,#15726);
#67=ITEM_DEFINED_TRANSFORMATION($,$,#15223,#15727);
#68=ITEM_DEFINED_TRANSFORMATION($,$,#15232,#15728);
#69=ITEM_DEFINED_TRANSFORMATION($,$,#15241,#15729);
#70=ITEM_DEFINED_TRANSFORMATION($,$,#15250,#15730);
#71=ITEM_DEFINED_TRANSFORMATION($,$,#15259,#15731);
#72=ITEM_DEFINED_TRANSFORMATION($,$,#15418,#15732);
#73=ITEM_DEFINED_TRANSFORMATION($,$,#15418,#15733);
#74=ITEM_DEFINED_TRANSFORMATION($,$,#15470,#15734);
#75=ITEM_DEFINED_TRANSFORMATION($,$,#15673,#15735);
#76=ITEM_DEFINED_TRANSFORMATION($,$,#15673,#15736);
#77=ITEM_DEFINED_TRANSFORMATION($,$,#15269,#15737);
#78=ITEM_DEFINED_TRANSFORMATION($,$,#15285,#15738);
#79=ITEM_DEFINED_TRANSFORMATION($,$,#15309,#15739);
#80=ITEM_DEFINED_TRANSFORMATION($,$,#15333,#15740);
#81=ITEM_DEFINED_TRANSFORMATION($,$,#15350,#15741);
#82=ITEM_DEFINED_TRANSFORMATION($,$,#15364,#15742);
#83=ITEM_DEFINED_TRANSFORMATION($,$,#15373,#15743);
#84=ITEM_DEFINED_TRANSFORMATION($,$,#15382,#15744);
#85=ITEM_DEFINED_TRANSFORMATION($,$,#15391,#15745);
#86=ITEM_DEFINED_TRANSFORMATION($,$,#15400,#15746);
#87=ITEM_DEFINED_TRANSFORMATION($,$,#15409,#15747);
#88=ITEM_DEFINED_TRANSFORMATION($,$,#15418,#15748);
#89=ITEM_DEFINED_TRANSFORMATION($,$,#15418,#15749);
#90=ITEM_DEFINED_TRANSFORMATION($,$,#15470,#15750);
#91=ITEM_DEFINED_TRANSFORMATION($,$,#15673,#15751);
#92=ITEM_DEFINED_TRANSFORMATION($,$,#15673,#15752);
#93=ITEM_DEFINED_TRANSFORMATION($,$,#15486,#15753);
#94=ITEM_DEFINED_TRANSFORMATION($,$,#15514,#15754);
#95=ITEM_DEFINED_TRANSFORMATION($,$,#15523,#15755);
#96=ITEM_DEFINED_TRANSFORMATION($,$,#15532,#15756);
#97=ITEM_DEFINED_TRANSFORMATION($,$,#15541,#15757);
#98=ITEM_DEFINED_TRANSFORMATION($,$,#15569,#15758);
#99=ITEM_DEFINED_TRANSFORMATION($,$,#15578,#15759);
#100=ITEM_DEFINED_TRANSFORMATION($,$,#15587,#15760);
#101=ITEM_DEFINED_TRANSFORMATION($,$,#15596,#15761);
#102=ITEM_DEFINED_TRANSFORMATION($,$,#15610,#15762);
#103=ITEM_DEFINED_TRANSFORMATION($,$,#15619,#15763);
#104=ITEM_DEFINED_TRANSFORMATION($,$,#15628,#15764);
#105=ITEM_DEFINED_TRANSFORMATION($,$,#15637,#15765);
#106=ITEM_DEFINED_TRANSFORMATION($,$,#15646,#15766);
#107=ITEM_DEFINED_TRANSFORMATION($,$,#15655,#15767);
#108=ITEM_DEFINED_TRANSFORMATION($,$,#15664,#15768);
#109=ITEM_DEFINED_TRANSFORMATION($,$,#15673,#15769);
#110=ITEM_DEFINED_TRANSFORMATION($,$,#15673,#15770);
#111=ITEM_DEFINED_TRANSFORMATION($,$,#16133,#16304);
#112=ITEM_DEFINED_TRANSFORMATION($,$,#16153,#16305);
#113=ITEM_DEFINED_TRANSFORMATION($,$,#16173,#16306);
#114=ITEM_DEFINED_TRANSFORMATION($,$,#16188,#16307);
#115=ITEM_DEFINED_TRANSFORMATION($,$,#16287,#16308);
#116=ITEM_DEFINED_TRANSFORMATION($,$,#14587,#16309);
#117=ITEM_DEFINED_TRANSFORMATION($,$,#14618,#16310);
#118=ITEM_DEFINED_TRANSFORMATION($,$,#14625,#16311);
#119=ITEM_DEFINED_TRANSFORMATION($,$,#14632,#16312);
#120=ITEM_DEFINED_TRANSFORMATION($,$,#14679,#16313);
#121=ITEM_DEFINED_TRANSFORMATION($,$,#14704,#16314);
#122=ITEM_DEFINED_TRANSFORMATION($,$,#14729,#16315);
#123=ITEM_DEFINED_TRANSFORMATION($,$,#14773,#16316);
#124=ITEM_DEFINED_TRANSFORMATION($,$,#14798,#16317);
#125=ITEM_DEFINED_TRANSFORMATION($,$,#14823,#16318);
#126=ITEM_DEFINED_TRANSFORMATION($,$,#14829,#16319);
#127=ITEM_DEFINED_TRANSFORMATION($,$,#14835,#16320);
#128=ITEM_DEFINED_TRANSFORMATION($,$,#14849,#16321);
#129=ITEM_DEFINED_TRANSFORMATION($,$,#14858,#16322);
#130=ITEM_DEFINED_TRANSFORMATION($,$,#14867,#16323);
#131=ITEM_DEFINED_TRANSFORMATION($,$,#14876,#16324);
#132=ITEM_DEFINED_TRANSFORMATION($,$,#14885,#16325);
#133=ITEM_DEFINED_TRANSFORMATION($,$,#15092,#16326);
#134=ITEM_DEFINED_TRANSFORMATION($,$,#15092,#16327);
#135=ITEM_DEFINED_TRANSFORMATION($,$,#15092,#16328);
#136=ITEM_DEFINED_TRANSFORMATION($,$,#15092,#16329);
#137=ITEM_DEFINED_TRANSFORMATION($,$,#16132,#16330);
#138=ITEM_DEFINED_TRANSFORMATION($,$,#14894,#16331);
#139=ITEM_DEFINED_TRANSFORMATION($,$,#14894,#16332);
#140=ITEM_DEFINED_TRANSFORMATION($,$,#14894,#16333);
#141=ITEM_DEFINED_TRANSFORMATION($,$,#14894,#16334);
#142=ITEM_DEFINED_TRANSFORMATION($,$,#14894,#16335);
#143=ITEM_DEFINED_TRANSFORMATION($,$,#14894,#16336);
#144=ITEM_DEFINED_TRANSFORMATION($,$,#14894,#16337);
#145=ITEM_DEFINED_TRANSFORMATION($,$,#14894,#16338);
#146=ITEM_DEFINED_TRANSFORMATION($,$,#15092,#16339);
#147=ITEM_DEFINED_TRANSFORMATION($,$,#15092,#16340);
#148=ITEM_DEFINED_TRANSFORMATION($,$,#15092,#16341);
#149=ITEM_DEFINED_TRANSFORMATION($,$,#15092,#16342);
#150=ITEM_DEFINED_TRANSFORMATION($,$,#16132,#16343);
#151=ITEM_DEFINED_TRANSFORMATION($,$,#14894,#16344);
#152=ITEM_DEFINED_TRANSFORMATION($,$,#14894,#16345);
#153=ITEM_DEFINED_TRANSFORMATION($,$,#14894,#16346);
#154=ITEM_DEFINED_TRANSFORMATION($,$,#14894,#16347);
#155=ITEM_DEFINED_TRANSFORMATION($,$,#14894,#16348);
#156=ITEM_DEFINED_TRANSFORMATION($,$,#14894,#16349);
#157=ITEM_DEFINED_TRANSFORMATION($,$,#14894,#16350);
#158=ITEM_DEFINED_TRANSFORMATION($,$,#14894,#16351);
#159=ITEM_DEFINED_TRANSFORMATION($,$,#15673,#16352);
#160=ITEM_DEFINED_TRANSFORMATION($,$,#15673,#16353);
#161=ITEM_DEFINED_TRANSFORMATION($,$,#15772,#16354);
#162=ITEM_DEFINED_TRANSFORMATION($,$,#15812,#16355);
#163=ITEM_DEFINED_TRANSFORMATION($,$,#15821,#16356);
#164=ITEM_DEFINED_TRANSFORMATION($,$,#15830,#16357);
#165=ITEM_DEFINED_TRANSFORMATION($,$,#15851,#16358);
#166=ITEM_DEFINED_TRANSFORMATION($,$,#15861,#16359);
#167=ITEM_DEFINED_TRANSFORMATION($,$,#15871,#16360);
#168=ITEM_DEFINED_TRANSFORMATION($,$,#15881,#16361);
#169=ITEM_DEFINED_TRANSFORMATION($,$,#15891,#16362);
#170=ITEM_DEFINED_TRANSFORMATION($,$,#15912,#16363);
#171=ITEM_DEFINED_TRANSFORMATION($,$,#15922,#16364);
#172=ITEM_DEFINED_TRANSFORMATION($,$,#15932,#16365);
#173=ITEM_DEFINED_TRANSFORMATION($,$,#15942,#16366);
#174=ITEM_DEFINED_TRANSFORMATION($,$,#15952,#16367);
#175=ITEM_DEFINED_TRANSFORMATION($,$,#15992,#16368);
#176=ITEM_DEFINED_TRANSFORMATION($,$,#16001,#16369);
#177=ITEM_DEFINED_TRANSFORMATION($,$,#16010,#16370);
#178=ITEM_DEFINED_TRANSFORMATION($,$,#16031,#16371);
#179=ITEM_DEFINED_TRANSFORMATION($,$,#16041,#16372);
#180=ITEM_DEFINED_TRANSFORMATION($,$,#16051,#16373);
#181=ITEM_DEFINED_TRANSFORMATION($,$,#16061,#16374);
#182=ITEM_DEFINED_TRANSFORMATION($,$,#16071,#16375);
#183=ITEM_DEFINED_TRANSFORMATION($,$,#16092,#16376);
#184=ITEM_DEFINED_TRANSFORMATION($,$,#16102,#16377);
#185=ITEM_DEFINED_TRANSFORMATION($,$,#16112,#16378);
#186=ITEM_DEFINED_TRANSFORMATION($,$,#16122,#16379);
#187=ITEM_DEFINED_TRANSFORMATION($,$,#16132,#16380);
#188=ITEM_DEFINED_TRANSFORMATION($,$,#16132,#16381);
#189=ITEM_DEFINED_TRANSFORMATION($,$,#16383,#16454);
#190=ITEM_DEFINED_TRANSFORMATION($,$,#16405,#16455);
#191=ITEM_DEFINED_TRANSFORMATION($,$,#16414,#16456);
#192=ITEM_DEFINED_TRANSFORMATION($,$,#16423,#16457);
#193=ITEM_DEFINED_TRANSFORMATION($,$,#16432,#16458);
#194=ITEM_DEFINED_TRANSFORMATION($,$,#16441,#16459);
#195=ITEM_DEFINED_TRANSFORMATION($,$,#14586,#16460);
#196=ITEM_DEFINED_TRANSFORMATION($,$,#14918,#16461);
#197=ITEM_DEFINED_TRANSFORMATION($,$,#15118,#16462);
#198=ITEM_DEFINED_TRANSFORMATION($,$,#15268,#16463);
#199=ITEM_DEFINED_TRANSFORMATION($,$,#15485,#16464);
#200=ITEM_DEFINED_TRANSFORMATION($,$,#15771,#16465);
#201=ITEM_DEFINED_TRANSFORMATION($,$,#16382,#16466);
#202=(
REPRESENTATION_RELATIONSHIP($,$,#25569,#25568)
REPRESENTATION_RELATIONSHIP_WITH_TRANSFORMATION(#37)
SHAPE_REPRESENTATION_RELATIONSHIP()
);
#203=(
REPRESENTATION_RELATIONSHIP($,$,#25570,#25568)
REPRESENTATION_RELATIONSHIP_WITH_TRANSFORMATION(#38)
SHAPE_REPRESENTATION_RELATIONSHIP()
);
#204=(
REPRESENTATION_RELATIONSHIP($,$,#25531,#25530)
REPRESENTATION_RELATIONSHIP_WITH_TRANSFORMATION(#39)
SHAPE_REPRESENTATION_RELATIONSHIP()
);
#205=(
REPRESENTATION_RELATIONSHIP($,$,#25532,#25530)
REPRESENTATION_RELATIONSHIP_WITH_TRANSFORMATION(#40)
SHAPE_REPRESENTATION_RELATIONSHIP()
);
#206=(
REPRESENTATION_RELATIONSHIP($,$,#25533,#25530)
REPRESENTATION_RELATIONSHIP_WITH_TRANSFORMATION(#41)
SHAPE_REPRESENTATION_RELATIONSHIP()
);
#207=(
REPRESENTATION_RELATIONSHIP($,$,#25534,#25530)
REPRESENTATION_RELATIONSHIP_WITH_TRANSFORMATION(#42)
SHAPE_REPRESENTATION_RELATIONSHIP()
);
#208=(
REPRESENTATION_RELATIONSHIP($,$,#25535,#25530)
REPRESENTATION_RELATIONSHIP_WITH_TRANSFORMATION(#43)
SHAPE_REPRESENTATION_RELATIONSHIP()
);
#209=(
REPRESENTATION_RELATIONSHIP($,$,#25536,#25530)
REPRESENTATION_RELATIONSHIP_WITH_TRANSFORMATION(#44)
SHAPE_REPRESENTATION_RELATIONSHIP()
);
#210=(
REPRESENTATION_RELATIONSHIP($,$,#25537,#25530)
REPRESENTATION_RELATIONSHIP_WITH_TRANSFORMATION(#45)
SHAPE_REPRESENTATION_RELATIONSHIP()
);
#211=(
REPRESENTATION_RELATIONSHIP($,$,#25538,#25530)
REPRESENTATION_RELATIONSHIP_WITH_TRANSFORMATION(#46)
SHAPE_REPRESENTATION_RELATIONSHIP()
);
#212=(
REPRESENTATION_RELATIONSHIP($,$,#25539,#25530)
REPRESENTATION_RELATIONSHIP_WITH_TRANSFORMATION(#47)
SHAPE_REPRESENTATION_RELATIONSHIP()
);
#213=(
REPRESENTATION_RELATIONSHIP($,$,#25540,#25530)
REPRESENTATION_RELATIONSHIP_WITH_TRANSFORMATION(#48)
SHAPE_REPRESENTATION_RELATIONSHIP()
);
#214=(
REPRESENTATION_RELATIONSHIP($,$,#25541,#25530)
REPRESENTATION_RELATIONSHIP_WITH_TRANSFORMATION(#49)
SHAPE_REPRESENTATION_RELATIONSHIP()
);
#215=(
REPRESENTATION_RELATIONSHIP($,$,#25542,#25530)
REPRESENTATION_RELATIONSHIP_WITH_TRANSFORMATION(#50)
SHAPE_REPRESENTATION_RELATIONSHIP()
);
#216=(
REPRESENTATION_RELATIONSHIP($,$,#25543,#25530)
REPRESENTATION_RELATIONSHIP_WITH_TRANSFORMATION(#51)
SHAPE_REPRESENTATION_RELATIONSHIP()
);
#217=(
REPRESENTATION_RELATIONSHIP($,$,#25543,#25530)
REPRESENTATION_RELATIONSHIP_WITH_TRANSFORMATION(#52)
SHAPE_REPRESENTATION_RELATIONSHIP()
);
#218=(
REPRESENTATION_RELATIONSHIP($,$,#25543,#25530)
REPRESENTATION_RELATIONSHIP_WITH_TRANSFORMATION(#53)
SHAPE_REPRESENTATION_RELATIONSHIP()
);
#219=(
REPRESENTATION_RELATIONSHIP($,$,#25543,#25530)
REPRESENTATION_RELATIONSHIP_WITH_TRANSFORMATION(#54)
SHAPE_REPRESENTATION_RELATIONSHIP()
);
#220=(
REPRESENTATION_RELATIONSHIP($,$,#25543,#25530)
REPRESENTATION_RELATIONSHIP_WITH_TRANSFORMATION(#55)
SHAPE_REPRESENTATION_RELATIONSHIP()
);
#221=(
REPRESENTATION_RELATIONSHIP($,$,#25543,#25530)
REPRESENTATION_RELATIONSHIP_WITH_TRANSFORMATION(#56)
SHAPE_REPRESENTATION_RELATIONSHIP()
);
#222=(
REPRESENTATION_RELATIONSHIP($,$,#25543,#25530)
REPRESENTATION_RELATIONSHIP_WITH_TRANSFORMATION(#57)
SHAPE_REPRESENTATION_RELATIONSHIP()
);
#223=(
REPRESENTATION_RELATIONSHIP($,$,#25543,#25530)
REPRESENTATION_RELATIONSHIP_WITH_TRANSFORMATION(#58)
SHAPE_REPRESENTATION_RELATIONSHIP()
);
#224=(
REPRESENTATION_RELATIONSHIP($,$,#25589,#25530)
REPRESENTATION_RELATIONSHIP_WITH_TRANSFORMATION(#59)
SHAPE_REPRESENTATION_RELATIONSHIP()
);
#225=(
REPRESENTATION_RELATIONSHIP($,$,#25589,#25530)
REPRESENTATION_RELATIONSHIP_WITH_TRANSFORMATION(#60)
SHAPE_REPRESENTATION_RELATIONSHIP()
);
#226=(
REPRESENTATION_RELATIONSHIP($,$,#25545,#25544)
REPRESENTATION_RELATIONSHIP_WITH_TRANSFORMATION(#61)
SHAPE_REPRESENTATION_RELATIONSHIP()
);
#227=(
REPRESENTATION_RELATIONSHIP($,$,#25546,#25544)
REPRESENTATION_RELATIONSHIP_WITH_TRANSFORMATION(#62)
SHAPE_REPRESENTATION_RELATIONSHIP()
);
#228=(
REPRESENTATION_RELATIONSHIP($,$,#25547,#25544)
REPRESENTATION_RELATIONSHIP_WITH_TRANSFORMATION(#63)
SHAPE_REPRESENTATION_RELATIONSHIP()
);
#229=(
REPRESENTATION_RELATIONSHIP($,$,#25548,#25544)
REPRESENTATION_RELATIONSHIP_WITH_TRANSFORMATION(#64)
SHAPE_REPRESENTATION_RELATIONSHIP()
);
#230=(
REPRESENTATION_RELATIONSHIP($,$,#25549,#25544)
REPRESENTATION_RELATIONSHIP_WITH_TRANSFORMATION(#65)
SHAPE_REPRESENTATION_RELATIONSHIP()
);
#231=(
REPRESENTATION_RELATIONSHIP($,$,#25550,#25544)
REPRESENTATION_RELATIONSHIP_WITH_TRANSFORMATION(#66)
SHAPE_REPRESENTATION_RELATIONSHIP()
);
#232=(
REPRESENTATION_RELATIONSHIP($,$,#25551,#25544)
REPRESENTATION_RELATIONSHIP_WITH_TRANSFORMATION(#67)
SHAPE_REPRESENTATION_RELATIONSHIP()
);
#233=(
REPRESENTATION_RELATIONSHIP($,$,#25552,#25544)
REPRESENTATION_RELATIONSHIP_WITH_TRANSFORMATION(#68)
SHAPE_REPRESENTATION_RELATIONSHIP()
);
#234=(
REPRESENTATION_RELATIONSHIP($,$,#25553,#25544)
REPRESENTATION_RELATIONSHIP_WITH_TRANSFORMATION(#69)
SHAPE_REPRESENTATION_RELATIONSHIP()
);
#235=(
REPRESENTATION_RELATIONSHIP($,$,#25554,#25544)
REPRESENTATION_RELATIONSHIP_WITH_TRANSFORMATION(#70)
SHAPE_REPRESENTATION_RELATIONSHIP()
);
#236=(
REPRESENTATION_RELATIONSHIP($,$,#25555,#25544)
REPRESENTATION_RELATIONSHIP_WITH_TRANSFORMATION(#71)
SHAPE_REPRESENTATION_RELATIONSHIP()
);
#237=(
REPRESENTATION_RELATIONSHIP($,$,#25568,#25544)
REPRESENTATION_RELATIONSHIP_WITH_TRANSFORMATION(#72)
SHAPE_REPRESENTATION_RELATIONSHIP()
);
#238=(
REPRESENTATION_RELATIONSHIP($,$,#25568,#25544)
REPRESENTATION_RELATIONSHIP_WITH_TRANSFORMATION(#73)
SHAPE_REPRESENTATION_RELATIONSHIP()
);
#239=(
REPRESENTATION_RELATIONSHIP($,$,#25571,#25544)
REPRESENTATION_RELATIONSHIP_WITH_TRANSFORMATION(#74)
SHAPE_REPRESENTATION_RELATIONSHIP()
);
#240=(
REPRESENTATION_RELATIONSHIP($,$,#25589,#25544)
REPRESENTATION_RELATIONSHIP_WITH_TRANSFORMATION(#75)
SHAPE_REPRESENTATION_RELATIONSHIP()
);
#241=(
REPRESENTATION_RELATIONSHIP($,$,#25589,#25544)
REPRESENTATION_RELATIONSHIP_WITH_TRANSFORMATION(#76)
SHAPE_REPRESENTATION_RELATIONSHIP()
);
#242=(
REPRESENTATION_RELATIONSHIP($,$,#25557,#25556)
REPRESENTATION_RELATIONSHIP_WITH_TRANSFORMATION(#77)
SHAPE_REPRESENTATION_RELATIONSHIP()
);
#243=(
REPRESENTATION_RELATIONSHIP($,$,#25558,#25556)
REPRESENTATION_RELATIONSHIP_WITH_TRANSFORMATION(#78)
SHAPE_REPRESENTATION_RELATIONSHIP()
);
#244=(
REPRESENTATION_RELATIONSHIP($,$,#25559,#25556)
REPRESENTATION_RELATIONSHIP_WITH_TRANSFORMATION(#79)
SHAPE_REPRESENTATION_RELATIONSHIP()
);
#245=(
REPRESENTATION_RELATIONSHIP($,$,#25560,#25556)
REPRESENTATION_RELATIONSHIP_WITH_TRANSFORMATION(#80)
SHAPE_REPRESENTATION_RELATIONSHIP()
);
#246=(
REPRESENTATION_RELATIONSHIP($,$,#25561,#25556)
REPRESENTATION_RELATIONSHIP_WITH_TRANSFORMATION(#81)
SHAPE_REPRESENTATION_RELATIONSHIP()
);
#247=(
REPRESENTATION_RELATIONSHIP($,$,#25562,#25556)
REPRESENTATION_RELATIONSHIP_WITH_TRANSFORMATION(#82)
SHAPE_REPRESENTATION_RELATIONSHIP()
);
#248=(
REPRESENTATION_RELATIONSHIP($,$,#25563,#25556)
REPRESENTATION_RELATIONSHIP_WITH_TRANSFORMATION(#83)
SHAPE_REPRESENTATION_RELATIONSHIP()
);
#249=(
REPRESENTATION_RELATIONSHIP($,$,#25564,#25556)
REPRESENTATION_RELATIONSHIP_WITH_TRANSFORMATION(#84)
SHAPE_REPRESENTATION_RELATIONSHIP()
);
#250=(
REPRESENTATION_RELATIONSHIP($,$,#25565,#25556)
REPRESENTATION_RELATIONSHIP_WITH_TRANSFORMATION(#85)
SHAPE_REPRESENTATION_RELATIONSHIP()
);
#251=(
REPRESENTATION_RELATIONSHIP($,$,#25566,#25556)
REPRESENTATION_RELATIONSHIP_WITH_TRANSFORMATION(#86)
SHAPE_REPRESENTATION_RELATIONSHIP()
);
#252=(
REPRESENTATION_RELATIONSHIP($,$,#25567,#25556)
REPRESENTATION_RELATIONSHIP_WITH_TRANSFORMATION(#87)
SHAPE_REPRESENTATION_RELATIONSHIP()
);
#253=(
REPRESENTATION_RELATIONSHIP($,$,#25568,#25556)
REPRESENTATION_RELATIONSHIP_WITH_TRANSFORMATION(#88)
SHAPE_REPRESENTATION_RELATIONSHIP()
);
#254=(
REPRESENTATION_RELATIONSHIP($,$,#25568,#25556)
REPRESENTATION_RELATIONSHIP_WITH_TRANSFORMATION(#89)
SHAPE_REPRESENTATION_RELATIONSHIP()
);
#255=(
REPRESENTATION_RELATIONSHIP($,$,#25571,#25556)
REPRESENTATION_RELATIONSHIP_WITH_TRANSFORMATION(#90)
SHAPE_REPRESENTATION_RELATIONSHIP()
);
#256=(
REPRESENTATION_RELATIONSHIP($,$,#25589,#25556)
REPRESENTATION_RELATIONSHIP_WITH_TRANSFORMATION(#91)
SHAPE_REPRESENTATION_RELATIONSHIP()
);
#257=(
REPRESENTATION_RELATIONSHIP($,$,#25589,#25556)
REPRESENTATION_RELATIONSHIP_WITH_TRANSFORMATION(#92)
SHAPE_REPRESENTATION_RELATIONSHIP()
);
#258=(
REPRESENTATION_RELATIONSHIP($,$,#25573,#25572)
REPRESENTATION_RELATIONSHIP_WITH_TRANSFORMATION(#93)
SHAPE_REPRESENTATION_RELATIONSHIP()
);
#259=(
REPRESENTATION_RELATIONSHIP($,$,#25574,#25572)
REPRESENTATION_RELATIONSHIP_WITH_TRANSFORMATION(#94)
SHAPE_REPRESENTATION_RELATIONSHIP()
);
#260=(
REPRESENTATION_RELATIONSHIP($,$,#25575,#25572)
REPRESENTATION_RELATIONSHIP_WITH_TRANSFORMATION(#95)
SHAPE_REPRESENTATION_RELATIONSHIP()
);
#261=(
REPRESENTATION_RELATIONSHIP($,$,#25576,#25572)
REPRESENTATION_RELATIONSHIP_WITH_TRANSFORMATION(#96)
SHAPE_REPRESENTATION_RELATIONSHIP()
);
#262=(
REPRESENTATION_RELATIONSHIP($,$,#25577,#25572)
REPRESENTATION_RELATIONSHIP_WITH_TRANSFORMATION(#97)
SHAPE_REPRESENTATION_RELATIONSHIP()
);
#263=(
REPRESENTATION_RELATIONSHIP($,$,#25578,#25572)
REPRESENTATION_RELATIONSHIP_WITH_TRANSFORMATION(#98)
SHAPE_REPRESENTATION_RELATIONSHIP()
);
#264=(
REPRESENTATION_RELATIONSHIP($,$,#25579,#25572)
REPRESENTATION_RELATIONSHIP_WITH_TRANSFORMATION(#99)
SHAPE_REPRESENTATION_RELATIONSHIP()
);
#265=(
REPRESENTATION_RELATIONSHIP($,$,#25580,#25572)
REPRESENTATION_RELATIONSHIP_WITH_TRANSFORMATION(#100)
SHAPE_REPRESENTATION_RELATIONSHIP()
);
#266=(
REPRESENTATION_RELATIONSHIP($,$,#25581,#25572)
REPRESENTATION_RELATIONSHIP_WITH_TRANSFORMATION(#101)
SHAPE_REPRESENTATION_RELATIONSHIP()
);
#267=(
REPRESENTATION_RELATIONSHIP($,$,#25582,#25572)
REPRESENTATION_RELATIONSHIP_WITH_TRANSFORMATION(#102)
SHAPE_REPRESENTATION_RELATIONSHIP()
);
#268=(
REPRESENTATION_RELATIONSHIP($,$,#25583,#25572)
REPRESENTATION_RELATIONSHIP_WITH_TRANSFORMATION(#103)
SHAPE_REPRESENTATION_RELATIONSHIP()
);
#269=(
REPRESENTATION_RELATIONSHIP($,$,#25584,#25572)
REPRESENTATION_RELATIONSHIP_WITH_TRANSFORMATION(#104)
SHAPE_REPRESENTATION_RELATIONSHIP()
);
#270=(
REPRESENTATION_RELATIONSHIP($,$,#25585,#25572)
REPRESENTATION_RELATIONSHIP_WITH_TRANSFORMATION(#105)
SHAPE_REPRESENTATION_RELATIONSHIP()
);
#271=(
REPRESENTATION_RELATIONSHIP($,$,#25586,#25572)
REPRESENTATION_RELATIONSHIP_WITH_TRANSFORMATION(#106)
SHAPE_REPRESENTATION_RELATIONSHIP()
);
#272=(
REPRESENTATION_RELATIONSHIP($,$,#25587,#25572)
REPRESENTATION_RELATIONSHIP_WITH_TRANSFORMATION(#107)
SHAPE_REPRESENTATION_RELATIONSHIP()
);
#273=(
REPRESENTATION_RELATIONSHIP($,$,#25588,#25572)
REPRESENTATION_RELATIONSHIP_WITH_TRANSFORMATION(#108)
SHAPE_REPRESENTATION_RELATIONSHIP()
);
#274=(
REPRESENTATION_RELATIONSHIP($,$,#25589,#25572)
REPRESENTATION_RELATIONSHIP_WITH_TRANSFORMATION(#109)
SHAPE_REPRESENTATION_RELATIONSHIP()
);
#275=(
REPRESENTATION_RELATIONSHIP($,$,#25589,#25572)
REPRESENTATION_RELATIONSHIP_WITH_TRANSFORMATION(#110)
SHAPE_REPRESENTATION_RELATIONSHIP()
);
#276=(
REPRESENTATION_RELATIONSHIP($,$,#25618,#25617)
REPRESENTATION_RELATIONSHIP_WITH_TRANSFORMATION(#111)
SHAPE_REPRESENTATION_RELATIONSHIP()
);
#277=(
REPRESENTATION_RELATIONSHIP($,$,#25619,#25617)
REPRESENTATION_RELATIONSHIP_WITH_TRANSFORMATION(#112)
SHAPE_REPRESENTATION_RELATIONSHIP()
);
#278=(
REPRESENTATION_RELATIONSHIP($,$,#25620,#25617)
REPRESENTATION_RELATIONSHIP_WITH_TRANSFORMATION(#113)
SHAPE_REPRESENTATION_RELATIONSHIP()
);
#279=(
REPRESENTATION_RELATIONSHIP($,$,#25621,#25617)
REPRESENTATION_RELATIONSHIP_WITH_TRANSFORMATION(#114)
SHAPE_REPRESENTATION_RELATIONSHIP()
);
#280=(
REPRESENTATION_RELATIONSHIP($,$,#25622,#25617)
REPRESENTATION_RELATIONSHIP_WITH_TRANSFORMATION(#115)
SHAPE_REPRESENTATION_RELATIONSHIP()
);
#281=(
REPRESENTATION_RELATIONSHIP($,$,#25512,#25511)
REPRESENTATION_RELATIONSHIP_WITH_TRANSFORMATION(#116)
SHAPE_REPRESENTATION_RELATIONSHIP()
);
#282=(
REPRESENTATION_RELATIONSHIP($,$,#25513,#25511)
REPRESENTATION_RELATIONSHIP_WITH_TRANSFORMATION(#117)
SHAPE_REPRESENTATION_RELATIONSHIP()
);
#283=(
REPRESENTATION_RELATIONSHIP($,$,#25514,#25511)
REPRESENTATION_RELATIONSHIP_WITH_TRANSFORMATION(#118)
SHAPE_REPRESENTATION_RELATIONSHIP()
);
#284=(
REPRESENTATION_RELATIONSHIP($,$,#25515,#25511)
REPRESENTATION_RELATIONSHIP_WITH_TRANSFORMATION(#119)
SHAPE_REPRESENTATION_RELATIONSHIP()
);
#285=(
REPRESENTATION_RELATIONSHIP($,$,#25516,#25511)
REPRESENTATION_RELATIONSHIP_WITH_TRANSFORMATION(#120)
SHAPE_REPRESENTATION_RELATIONSHIP()
);
#286=(
REPRESENTATION_RELATIONSHIP($,$,#25517,#25511)
REPRESENTATION_RELATIONSHIP_WITH_TRANSFORMATION(#121)
SHAPE_REPRESENTATION_RELATIONSHIP()
);
#287=(
REPRESENTATION_RELATIONSHIP($,$,#25518,#25511)
REPRESENTATION_RELATIONSHIP_WITH_TRANSFORMATION(#122)
SHAPE_REPRESENTATION_RELATIONSHIP()
);
#288=(
REPRESENTATION_RELATIONSHIP($,$,#25519,#25511)
REPRESENTATION_RELATIONSHIP_WITH_TRANSFORMATION(#123)
SHAPE_REPRESENTATION_RELATIONSHIP()
);
#289=(
REPRESENTATION_RELATIONSHIP($,$,#25520,#25511)
REPRESENTATION_RELATIONSHIP_WITH_TRANSFORMATION(#124)
SHAPE_REPRESENTATION_RELATIONSHIP()
);
#290=(
REPRESENTATION_RELATIONSHIP($,$,#25521,#25511)
REPRESENTATION_RELATIONSHIP_WITH_TRANSFORMATION(#125)
SHAPE_REPRESENTATION_RELATIONSHIP()
);
#291=(
REPRESENTATION_RELATIONSHIP($,$,#25522,#25511)
REPRESENTATION_RELATIONSHIP_WITH_TRANSFORMATION(#126)
SHAPE_REPRESENTATION_RELATIONSHIP()
);
#292=(
REPRESENTATION_RELATIONSHIP($,$,#25523,#25511)
REPRESENTATION_RELATIONSHIP_WITH_TRANSFORMATION(#127)
SHAPE_REPRESENTATION_RELATIONSHIP()
);
#293=(
REPRESENTATION_RELATIONSHIP($,$,#25524,#25511)
REPRESENTATION_RELATIONSHIP_WITH_TRANSFORMATION(#128)
SHAPE_REPRESENTATION_RELATIONSHIP()
);
#294=(
REPRESENTATION_RELATIONSHIP($,$,#25525,#25511)
REPRESENTATION_RELATIONSHIP_WITH_TRANSFORMATION(#129)
SHAPE_REPRESENTATION_RELATIONSHIP()
);
#295=(
REPRESENTATION_RELATIONSHIP($,$,#25526,#25511)
REPRESENTATION_RELATIONSHIP_WITH_TRANSFORMATION(#130)
SHAPE_REPRESENTATION_RELATIONSHIP()
);
#296=(
REPRESENTATION_RELATIONSHIP($,$,#25527,#25511)
REPRESENTATION_RELATIONSHIP_WITH_TRANSFORMATION(#131)
SHAPE_REPRESENTATION_RELATIONSHIP()
);
#297=(
REPRESENTATION_RELATIONSHIP($,$,#25528,#25511)
REPRESENTATION_RELATIONSHIP_WITH_TRANSFORMATION(#132)
SHAPE_REPRESENTATION_RELATIONSHIP()
);
#298=(
REPRESENTATION_RELATIONSHIP($,$,#25543,#25511)
REPRESENTATION_RELATIONSHIP_WITH_TRANSFORMATION(#133)
SHAPE_REPRESENTATION_RELATIONSHIP()
);
#299=(
REPRESENTATION_RELATIONSHIP($,$,#25543,#25511)
REPRESENTATION_RELATIONSHIP_WITH_TRANSFORMATION(#134)
SHAPE_REPRESENTATION_RELATIONSHIP()
);
#300=(
REPRESENTATION_RELATIONSHIP($,$,#25543,#25511)
REPRESENTATION_RELATIONSHIP_WITH_TRANSFORMATION(#135)
SHAPE_REPRESENTATION_RELATIONSHIP()
);
#301=(
REPRESENTATION_RELATIONSHIP($,$,#25543,#25511)
REPRESENTATION_RELATIONSHIP_WITH_TRANSFORMATION(#136)
SHAPE_REPRESENTATION_RELATIONSHIP()
);
#302=(
REPRESENTATION_RELATIONSHIP($,$,#25617,#25511)
REPRESENTATION_RELATIONSHIP_WITH_TRANSFORMATION(#137)
SHAPE_REPRESENTATION_RELATIONSHIP()
);
#303=(
REPRESENTATION_RELATIONSHIP($,$,#25529,#25511)
REPRESENTATION_RELATIONSHIP_WITH_TRANSFORMATION(#138)
SHAPE_REPRESENTATION_RELATIONSHIP()
);
#304=(
REPRESENTATION_RELATIONSHIP($,$,#25529,#25511)
REPRESENTATION_RELATIONSHIP_WITH_TRANSFORMATION(#139)
SHAPE_REPRESENTATION_RELATIONSHIP()
);
#305=(
REPRESENTATION_RELATIONSHIP($,$,#25529,#25511)
REPRESENTATION_RELATIONSHIP_WITH_TRANSFORMATION(#140)
SHAPE_REPRESENTATION_RELATIONSHIP()
);
#306=(
REPRESENTATION_RELATIONSHIP($,$,#25529,#25511)
REPRESENTATION_RELATIONSHIP_WITH_TRANSFORMATION(#141)
SHAPE_REPRESENTATION_RELATIONSHIP()
);
#307=(
REPRESENTATION_RELATIONSHIP($,$,#25529,#25511)
REPRESENTATION_RELATIONSHIP_WITH_TRANSFORMATION(#142)
SHAPE_REPRESENTATION_RELATIONSHIP()
);
#308=(
REPRESENTATION_RELATIONSHIP($,$,#25529,#25511)
REPRESENTATION_RELATIONSHIP_WITH_TRANSFORMATION(#143)
SHAPE_REPRESENTATION_RELATIONSHIP()
);
#309=(
REPRESENTATION_RELATIONSHIP($,$,#25529,#25511)
REPRESENTATION_RELATIONSHIP_WITH_TRANSFORMATION(#144)
SHAPE_REPRESENTATION_RELATIONSHIP()
);
#310=(
REPRESENTATION_RELATIONSHIP($,$,#25529,#25511)
REPRESENTATION_RELATIONSHIP_WITH_TRANSFORMATION(#145)
SHAPE_REPRESENTATION_RELATIONSHIP()
);
#311=(
REPRESENTATION_RELATIONSHIP($,$,#25543,#25511)
REPRESENTATION_RELATIONSHIP_WITH_TRANSFORMATION(#146)
SHAPE_REPRESENTATION_RELATIONSHIP()
);
#312=(
REPRESENTATION_RELATIONSHIP($,$,#25543,#25511)
REPRESENTATION_RELATIONSHIP_WITH_TRANSFORMATION(#147)
SHAPE_REPRESENTATION_RELATIONSHIP()
);
#313=(
REPRESENTATION_RELATIONSHIP($,$,#25543,#25511)
REPRESENTATION_RELATIONSHIP_WITH_TRANSFORMATION(#148)
SHAPE_REPRESENTATION_RELATIONSHIP()
);
#314=(
REPRESENTATION_RELATIONSHIP($,$,#25543,#25511)
REPRESENTATION_RELATIONSHIP_WITH_TRANSFORMATION(#149)
SHAPE_REPRESENTATION_RELATIONSHIP()
);
#315=(
REPRESENTATION_RELATIONSHIP($,$,#25617,#25511)
REPRESENTATION_RELATIONSHIP_WITH_TRANSFORMATION(#150)
SHAPE_REPRESENTATION_RELATIONSHIP()
);
#316=(
REPRESENTATION_RELATIONSHIP($,$,#25529,#25511)
REPRESENTATION_RELATIONSHIP_WITH_TRANSFORMATION(#151)
SHAPE_REPRESENTATION_RELATIONSHIP()
);
#317=(
REPRESENTATION_RELATIONSHIP($,$,#25529,#25511)
REPRESENTATION_RELATIONSHIP_WITH_TRANSFORMATION(#152)
SHAPE_REPRESENTATION_RELATIONSHIP()
);
#318=(
REPRESENTATION_RELATIONSHIP($,$,#25529,#25511)
REPRESENTATION_RELATIONSHIP_WITH_TRANSFORMATION(#153)
SHAPE_REPRESENTATION_RELATIONSHIP()
);
#319=(
REPRESENTATION_RELATIONSHIP($,$,#25529,#25511)
REPRESENTATION_RELATIONSHIP_WITH_TRANSFORMATION(#154)
SHAPE_REPRESENTATION_RELATIONSHIP()
);
#320=(
REPRESENTATION_RELATIONSHIP($,$,#25529,#25511)
REPRESENTATION_RELATIONSHIP_WITH_TRANSFORMATION(#155)
SHAPE_REPRESENTATION_RELATIONSHIP()
);
#321=(
REPRESENTATION_RELATIONSHIP($,$,#25529,#25511)
REPRESENTATION_RELATIONSHIP_WITH_TRANSFORMATION(#156)
SHAPE_REPRESENTATION_RELATIONSHIP()
);
#322=(
REPRESENTATION_RELATIONSHIP($,$,#25529,#25511)
REPRESENTATION_RELATIONSHIP_WITH_TRANSFORMATION(#157)
SHAPE_REPRESENTATION_RELATIONSHIP()
);
#323=(
REPRESENTATION_RELATIONSHIP($,$,#25529,#25511)
REPRESENTATION_RELATIONSHIP_WITH_TRANSFORMATION(#158)
SHAPE_REPRESENTATION_RELATIONSHIP()
);
#324=(
REPRESENTATION_RELATIONSHIP($,$,#25589,#25511)
REPRESENTATION_RELATIONSHIP_WITH_TRANSFORMATION(#159)
SHAPE_REPRESENTATION_RELATIONSHIP()
);
#325=(
REPRESENTATION_RELATIONSHIP($,$,#25589,#25511)
REPRESENTATION_RELATIONSHIP_WITH_TRANSFORMATION(#160)
SHAPE_REPRESENTATION_RELATIONSHIP()
);
#326=(
REPRESENTATION_RELATIONSHIP($,$,#25591,#25590)
REPRESENTATION_RELATIONSHIP_WITH_TRANSFORMATION(#161)
SHAPE_REPRESENTATION_RELATIONSHIP()
);
#327=(
REPRESENTATION_RELATIONSHIP($,$,#25592,#25590)
REPRESENTATION_RELATIONSHIP_WITH_TRANSFORMATION(#162)
SHAPE_REPRESENTATION_RELATIONSHIP()
);
#328=(
REPRESENTATION_RELATIONSHIP($,$,#25593,#25590)
REPRESENTATION_RELATIONSHIP_WITH_TRANSFORMATION(#163)
SHAPE_REPRESENTATION_RELATIONSHIP()
);
#329=(
REPRESENTATION_RELATIONSHIP($,$,#25594,#25590)
REPRESENTATION_RELATIONSHIP_WITH_TRANSFORMATION(#164)
SHAPE_REPRESENTATION_RELATIONSHIP()
);
#330=(
REPRESENTATION_RELATIONSHIP($,$,#25595,#25590)
REPRESENTATION_RELATIONSHIP_WITH_TRANSFORMATION(#165)
SHAPE_REPRESENTATION_RELATIONSHIP()
);
#331=(
REPRESENTATION_RELATIONSHIP($,$,#25596,#25590)
REPRESENTATION_RELATIONSHIP_WITH_TRANSFORMATION(#166)
SHAPE_REPRESENTATION_RELATIONSHIP()
);
#332=(
REPRESENTATION_RELATIONSHIP($,$,#25597,#25590)
REPRESENTATION_RELATIONSHIP_WITH_TRANSFORMATION(#167)
SHAPE_REPRESENTATION_RELATIONSHIP()
);
#333=(
REPRESENTATION_RELATIONSHIP($,$,#25598,#25590)
REPRESENTATION_RELATIONSHIP_WITH_TRANSFORMATION(#168)
SHAPE_REPRESENTATION_RELATIONSHIP()
);
#334=(
REPRESENTATION_RELATIONSHIP($,$,#25599,#25590)
REPRESENTATION_RELATIONSHIP_WITH_TRANSFORMATION(#169)
SHAPE_REPRESENTATION_RELATIONSHIP()
);
#335=(
REPRESENTATION_RELATIONSHIP($,$,#25600,#25590)
REPRESENTATION_RELATIONSHIP_WITH_TRANSFORMATION(#170)
SHAPE_REPRESENTATION_RELATIONSHIP()
);
#336=(
REPRESENTATION_RELATIONSHIP($,$,#25601,#25590)
REPRESENTATION_RELATIONSHIP_WITH_TRANSFORMATION(#171)
SHAPE_REPRESENTATION_RELATIONSHIP()
);
#337=(
REPRESENTATION_RELATIONSHIP($,$,#25602,#25590)
REPRESENTATION_RELATIONSHIP_WITH_TRANSFORMATION(#172)
SHAPE_REPRESENTATION_RELATIONSHIP()
);
#338=(
REPRESENTATION_RELATIONSHIP($,$,#25603,#25590)
REPRESENTATION_RELATIONSHIP_WITH_TRANSFORMATION(#173)
SHAPE_REPRESENTATION_RELATIONSHIP()
);
#339=(
REPRESENTATION_RELATIONSHIP($,$,#25604,#25590)
REPRESENTATION_RELATIONSHIP_WITH_TRANSFORMATION(#174)
SHAPE_REPRESENTATION_RELATIONSHIP()
);
#340=(
REPRESENTATION_RELATIONSHIP($,$,#25605,#25590)
REPRESENTATION_RELATIONSHIP_WITH_TRANSFORMATION(#175)
SHAPE_REPRESENTATION_RELATIONSHIP()
);
#341=(
REPRESENTATION_RELATIONSHIP($,$,#25606,#25590)
REPRESENTATION_RELATIONSHIP_WITH_TRANSFORMATION(#176)
SHAPE_REPRESENTATION_RELATIONSHIP()
);
#342=(
REPRESENTATION_RELATIONSHIP($,$,#25607,#25590)
REPRESENTATION_RELATIONSHIP_WITH_TRANSFORMATION(#177)
SHAPE_REPRESENTATION_RELATIONSHIP()
);
#343=(
REPRESENTATION_RELATIONSHIP($,$,#25608,#25590)
REPRESENTATION_RELATIONSHIP_WITH_TRANSFORMATION(#178)
SHAPE_REPRESENTATION_RELATIONSHIP()
);
#344=(
REPRESENTATION_RELATIONSHIP($,$,#25609,#25590)
REPRESENTATION_RELATIONSHIP_WITH_TRANSFORMATION(#179)
SHAPE_REPRESENTATION_RELATIONSHIP()
);
#345=(
REPRESENTATION_RELATIONSHIP($,$,#25610,#25590)
REPRESENTATION_RELATIONSHIP_WITH_TRANSFORMATION(#180)
SHAPE_REPRESENTATION_RELATIONSHIP()
);
#346=(
REPRESENTATION_RELATIONSHIP($,$,#25611,#25590)
REPRESENTATION_RELATIONSHIP_WITH_TRANSFORMATION(#181)
SHAPE_REPRESENTATION_RELATIONSHIP()
);
#347=(
REPRESENTATION_RELATIONSHIP($,$,#25612,#25590)
REPRESENTATION_RELATIONSHIP_WITH_TRANSFORMATION(#182)
SHAPE_REPRESENTATION_RELATIONSHIP()
);
#348=(
REPRESENTATION_RELATIONSHIP($,$,#25613,#25590)
REPRESENTATION_RELATIONSHIP_WITH_TRANSFORMATION(#183)
SHAPE_REPRESENTATION_RELATIONSHIP()
);
#349=(
REPRESENTATION_RELATIONSHIP($,$,#25614,#25590)
REPRESENTATION_RELATIONSHIP_WITH_TRANSFORMATION(#184)
SHAPE_REPRESENTATION_RELATIONSHIP()
);
#350=(
REPRESENTATION_RELATIONSHIP($,$,#25615,#25590)
REPRESENTATION_RELATIONSHIP_WITH_TRANSFORMATION(#185)
SHAPE_REPRESENTATION_RELATIONSHIP()
);
#351=(
REPRESENTATION_RELATIONSHIP($,$,#25616,#25590)
REPRESENTATION_RELATIONSHIP_WITH_TRANSFORMATION(#186)
SHAPE_REPRESENTATION_RELATIONSHIP()
);
#352=(
REPRESENTATION_RELATIONSHIP($,$,#25617,#25590)
REPRESENTATION_RELATIONSHIP_WITH_TRANSFORMATION(#187)
SHAPE_REPRESENTATION_RELATIONSHIP()
);
#353=(
REPRESENTATION_RELATIONSHIP($,$,#25617,#25590)
REPRESENTATION_RELATIONSHIP_WITH_TRANSFORMATION(#188)
SHAPE_REPRESENTATION_RELATIONSHIP()
);
#354=(
REPRESENTATION_RELATIONSHIP($,$,#25624,#25623)
REPRESENTATION_RELATIONSHIP_WITH_TRANSFORMATION(#189)
SHAPE_REPRESENTATION_RELATIONSHIP()
);
#355=(
REPRESENTATION_RELATIONSHIP($,$,#25625,#25623)
REPRESENTATION_RELATIONSHIP_WITH_TRANSFORMATION(#190)
SHAPE_REPRESENTATION_RELATIONSHIP()
);
#356=(
REPRESENTATION_RELATIONSHIP($,$,#25626,#25623)
REPRESENTATION_RELATIONSHIP_WITH_TRANSFORMATION(#191)
SHAPE_REPRESENTATION_RELATIONSHIP()
);
#357=(
REPRESENTATION_RELATIONSHIP($,$,#25627,#25623)
REPRESENTATION_RELATIONSHIP_WITH_TRANSFORMATION(#192)
SHAPE_REPRESENTATION_RELATIONSHIP()
);
#358=(
REPRESENTATION_RELATIONSHIP($,$,#25628,#25623)
REPRESENTATION_RELATIONSHIP_WITH_TRANSFORMATION(#193)
SHAPE_REPRESENTATION_RELATIONSHIP()
);
#359=(
REPRESENTATION_RELATIONSHIP($,$,#25629,#25623)
REPRESENTATION_RELATIONSHIP_WITH_TRANSFORMATION(#194)
SHAPE_REPRESENTATION_RELATIONSHIP()
);
#360=(
REPRESENTATION_RELATIONSHIP($,$,#25511,#25510)
REPRESENTATION_RELATIONSHIP_WITH_TRANSFORMATION(#195)
SHAPE_REPRESENTATION_RELATIONSHIP()
);
#361=(
REPRESENTATION_RELATIONSHIP($,$,#25530,#25510)
REPRESENTATION_RELATIONSHIP_WITH_TRANSFORMATION(#196)
SHAPE_REPRESENTATION_RELATIONSHIP()
);
#362=(
REPRESENTATION_RELATIONSHIP($,$,#25544,#25510)
REPRESENTATION_RELATIONSHIP_WITH_TRANSFORMATION(#197)
SHAPE_REPRESENTATION_RELATIONSHIP()
);
#363=(
REPRESENTATION_RELATIONSHIP($,$,#25556,#25510)
REPRESENTATION_RELATIONSHIP_WITH_TRANSFORMATION(#198)
SHAPE_REPRESENTATION_RELATIONSHIP()
);
#364=(
REPRESENTATION_RELATIONSHIP($,$,#25572,#25510)
REPRESENTATION_RELATIONSHIP_WITH_TRANSFORMATION(#199)
SHAPE_REPRESENTATION_RELATIONSHIP()
);
#365=(
REPRESENTATION_RELATIONSHIP($,$,#25590,#25510)
REPRESENTATION_RELATIONSHIP_WITH_TRANSFORMATION(#200)
SHAPE_REPRESENTATION_RELATIONSHIP()
);
#366=(
REPRESENTATION_RELATIONSHIP($,$,#25623,#25510)
REPRESENTATION_RELATIONSHIP_WITH_TRANSFORMATION(#201)
SHAPE_REPRESENTATION_RELATIONSHIP()
);
#367=CONTEXT_DEPENDENT_SHAPE_REPRESENTATION(#202,#25286);
#368=CONTEXT_DEPENDENT_SHAPE_REPRESENTATION(#203,#25287);
#369=CONTEXT_DEPENDENT_SHAPE_REPRESENTATION(#204,#25307);
#370=CONTEXT_DEPENDENT_SHAPE_REPRESENTATION(#205,#25308);
#371=CONTEXT_DEPENDENT_SHAPE_REPRESENTATION(#206,#25309);
#372=CONTEXT_DEPENDENT_SHAPE_REPRESENTATION(#207,#25310);
#373=CONTEXT_DEPENDENT_SHAPE_REPRESENTATION(#208,#25311);
#374=CONTEXT_DEPENDENT_SHAPE_REPRESENTATION(#209,#25312);
#375=CONTEXT_DEPENDENT_SHAPE_REPRESENTATION(#210,#25313);
#376=CONTEXT_DEPENDENT_SHAPE_REPRESENTATION(#211,#25314);
#377=CONTEXT_DEPENDENT_SHAPE_REPRESENTATION(#212,#25315);
#378=CONTEXT_DEPENDENT_SHAPE_REPRESENTATION(#213,#25316);
#379=CONTEXT_DEPENDENT_SHAPE_REPRESENTATION(#214,#25317);
#380=CONTEXT_DEPENDENT_SHAPE_REPRESENTATION(#215,#25318);
#381=CONTEXT_DEPENDENT_SHAPE_REPRESENTATION(#216,#25319);
#382=CONTEXT_DEPENDENT_SHAPE_REPRESENTATION(#217,#25320);
#383=CONTEXT_DEPENDENT_SHAPE_REPRESENTATION(#218,#25321);
#384=CONTEXT_DEPENDENT_SHAPE_REPRESENTATION(#219,#25322);
#385=CONTEXT_DEPENDENT_SHAPE_REPRESENTATION(#220,#25323);
#386=CONTEXT_DEPENDENT_SHAPE_REPRESENTATION(#221,#25324);
#387=CONTEXT_DEPENDENT_SHAPE_REPRESENTATION(#222,#25325);
#388=CONTEXT_DEPENDENT_SHAPE_REPRESENTATION(#223,#25326);
#389=CONTEXT_DEPENDENT_SHAPE_REPRESENTATION(#224,#25327);
#390=CONTEXT_DEPENDENT_SHAPE_REPRESENTATION(#225,#25328);
#391=CONTEXT_DEPENDENT_SHAPE_REPRESENTATION(#226,#25329);
#392=CONTEXT_DEPENDENT_SHAPE_REPRESENTATION(#227,#25330);
#393=CONTEXT_DEPENDENT_SHAPE_REPRESENTATION(#228,#25331);
#394=CONTEXT_DEPENDENT_SHAPE_REPRESENTATION(#229,#25332);
#395=CONTEXT_DEPENDENT_SHAPE_REPRESENTATION(#230,#25333);
#396=CONTEXT_DEPENDENT_SHAPE_REPRESENTATION(#231,#25334);
#397=CONTEXT_DEPENDENT_SHAPE_REPRESENTATION(#232,#25335);
#398=CONTEXT_DEPENDENT_SHAPE_REPRESENTATION(#233,#25336);
#399=CONTEXT_DEPENDENT_SHAPE_REPRESENTATION(#234,#25337);
#400=CONTEXT_DEPENDENT_SHAPE_REPRESENTATION(#235,#25338);
#401=CONTEXT_DEPENDENT_SHAPE_REPRESENTATION(#236,#25339);
#402=CONTEXT_DEPENDENT_SHAPE_REPRESENTATION(#237,#25340);
#403=CONTEXT_DEPENDENT_SHAPE_REPRESENTATION(#238,#25341);
#404=CONTEXT_DEPENDENT_SHAPE_REPRESENTATION(#239,#25342);
#405=CONTEXT_DEPENDENT_SHAPE_REPRESENTATION(#240,#25343);
#406=CONTEXT_DEPENDENT_SHAPE_REPRESENTATION(#241,#25344);
#407=CONTEXT_DEPENDENT_SHAPE_REPRESENTATION(#242,#25345);
#408=CONTEXT_DEPENDENT_SHAPE_REPRESENTATION(#243,#25346);
#409=CONTEXT_DEPENDENT_SHAPE_REPRESENTATION(#244,#25347);
#410=CONTEXT_DEPENDENT_SHAPE_REPRESENTATION(#245,#25348);
#411=CONTEXT_DEPENDENT_SHAPE_REPRESENTATION(#246,#25349);
#412=CONTEXT_DEPENDENT_SHAPE_REPRESENTATION(#247,#25350);
#413=CONTEXT_DEPENDENT_SHAPE_REPRESENTATION(#248,#25351);
#414=CONTEXT_DEPENDENT_SHAPE_REPRESENTATION(#249,#25352);
#415=CONTEXT_DEPENDENT_SHAPE_REPRESENTATION(#250,#25353);
#416=CONTEXT_DEPENDENT_SHAPE_REPRESENTATION(#251,#25354);
#417=CONTEXT_DEPENDENT_SHAPE_REPRESENTATION(#252,#25355);
#418=CONTEXT_DEPENDENT_SHAPE_REPRESENTATION(#253,#25356);
#419=CONTEXT_DEPENDENT_SHAPE_REPRESENTATION(#254,#25357);
#420=CONTEXT_DEPENDENT_SHAPE_REPRESENTATION(#255,#25358);
#421=CONTEXT_DEPENDENT_SHAPE_REPRESENTATION(#256,#25359);
#422=CONTEXT_DEPENDENT_SHAPE_REPRESENTATION(#257,#25360);
#423=CONTEXT_DEPENDENT_SHAPE_REPRESENTATION(#258,#25361);
#424=CONTEXT_DEPENDENT_SHAPE_REPRESENTATION(#259,#25362);
#425=CONTEXT_DEPENDENT_SHAPE_REPRESENTATION(#260,#25363);
#426=CONTEXT_DEPENDENT_SHAPE_REPRESENTATION(#261,#25364);
#427=CONTEXT_DEPENDENT_SHAPE_REPRESENTATION(#262,#25365);
#428=CONTEXT_DEPENDENT_SHAPE_REPRESENTATION(#263,#25366);
#429=CONTEXT_DEPENDENT_SHAPE_REPRESENTATION(#264,#25367);
#430=CONTEXT_DEPENDENT_SHAPE_REPRESENTATION(#265,#25368);
#431=CONTEXT_DEPENDENT_SHAPE_REPRESENTATION(#266,#25369);
#432=CONTEXT_DEPENDENT_SHAPE_REPRESENTATION(#267,#25370);
#433=CONTEXT_DEPENDENT_SHAPE_REPRESENTATION(#268,#25371);
#434=CONTEXT_DEPENDENT_SHAPE_REPRESENTATION(#269,#25372);
#435=CONTEXT_DEPENDENT_SHAPE_REPRESENTATION(#270,#25373);
#436=CONTEXT_DEPENDENT_SHAPE_REPRESENTATION(#271,#25374);
#437=CONTEXT_DEPENDENT_SHAPE_REPRESENTATION(#272,#25375);
#438=CONTEXT_DEPENDENT_SHAPE_REPRESENTATION(#273,#25376);
#439=CONTEXT_DEPENDENT_SHAPE_REPRESENTATION(#274,#25377);
#440=CONTEXT_DEPENDENT_SHAPE_REPRESENTATION(#275,#25378);
#441=CONTEXT_DEPENDENT_SHAPE_REPRESENTATION(#276,#25412);
#442=CONTEXT_DEPENDENT_SHAPE_REPRESENTATION(#277,#25413);
#443=CONTEXT_DEPENDENT_SHAPE_REPRESENTATION(#278,#25414);
#444=CONTEXT_DEPENDENT_SHAPE_REPRESENTATION(#279,#25415);
#445=CONTEXT_DEPENDENT_SHAPE_REPRESENTATION(#280,#25416);
#446=CONTEXT_DEPENDENT_SHAPE_REPRESENTATION(#281,#25417);
#447=CONTEXT_DEPENDENT_SHAPE_REPRESENTATION(#282,#25418);
#448=CONTEXT_DEPENDENT_SHAPE_REPRESENTATION(#283,#25419);
#449=CONTEXT_DEPENDENT_SHAPE_REPRESENTATION(#284,#25420);
#450=CONTEXT_DEPENDENT_SHAPE_REPRESENTATION(#285,#25421);
#451=CONTEXT_DEPENDENT_SHAPE_REPRESENTATION(#286,#25422);
#452=CONTEXT_DEPENDENT_SHAPE_REPRESENTATION(#287,#25423);
#453=CONTEXT_DEPENDENT_SHAPE_REPRESENTATION(#288,#25424);
#454=CONTEXT_DEPENDENT_SHAPE_REPRESENTATION(#289,#25425);
#455=CONTEXT_DEPENDENT_SHAPE_REPRESENTATION(#290,#25426);
#456=CONTEXT_DEPENDENT_SHAPE_REPRESENTATION(#291,#25427);
#457=CONTEXT_DEPENDENT_SHAPE_REPRESENTATION(#292,#25428);
#458=CONTEXT_DEPENDENT_SHAPE_REPRESENTATION(#293,#25429);
#459=CONTEXT_DEPENDENT_SHAPE_REPRESENTATION(#294,#25430);
#460=CONTEXT_DEPENDENT_SHAPE_REPRESENTATION(#295,#25431);
#461=CONTEXT_DEPENDENT_SHAPE_REPRESENTATION(#296,#25432);
#462=CONTEXT_DEPENDENT_SHAPE_REPRESENTATION(#297,#25433);
#463=CONTEXT_DEPENDENT_SHAPE_REPRESENTATION(#298,#25434);
#464=CONTEXT_DEPENDENT_SHAPE_REPRESENTATION(#299,#25435);
#465=CONTEXT_DEPENDENT_SHAPE_REPRESENTATION(#300,#25436);
#466=CONTEXT_DEPENDENT_SHAPE_REPRESENTATION(#301,#25437);
#467=CONTEXT_DEPENDENT_SHAPE_REPRESENTATION(#302,#25438);
#468=CONTEXT_DEPENDENT_SHAPE_REPRESENTATION(#303,#25439);
#469=CONTEXT_DEPENDENT_SHAPE_REPRESENTATION(#304,#25440);
#470=CONTEXT_DEPENDENT_SHAPE_REPRESENTATION(#305,#25441);
#471=CONTEXT_DEPENDENT_SHAPE_REPRESENTATION(#306,#25442);
#472=CONTEXT_DEPENDENT_SHAPE_REPRESENTATION(#307,#25443);
#473=CONTEXT_DEPENDENT_SHAPE_REPRESENTATION(#308,#25444);
#474=CONTEXT_DEPENDENT_SHAPE_REPRESENTATION(#309,#25445);
#475=CONTEXT_DEPENDENT_SHAPE_REPRESENTATION(#310,#25446);
#476=CONTEXT_DEPENDENT_SHAPE_REPRESENTATION(#311,#25447);
#477=CONTEXT_DEPENDENT_SHAPE_REPRESENTATION(#312,#25448);
#478=CONTEXT_DEPENDENT_SHAPE_REPRESENTATION(#313,#25449);
#479=CONTEXT_DEPENDENT_SHAPE_REPRESENTATION(#314,#25450);
#480=CONTEXT_DEPENDENT_SHAPE_REPRESENTATION(#315,#25451);
#481=CONTEXT_DEPENDENT_SHAPE_REPRESENTATION(#316,#25452);
#482=CONTEXT_DEPENDENT_SHAPE_REPRESENTATION(#317,#25453);
#483=CONTEXT_DEPENDENT_SHAPE_REPRESENTATION(#318,#25454);
#484=CONTEXT_DEPENDENT_SHAPE_REPRESENTATION(#319,#25455);
#485=CONTEXT_DEPENDENT_SHAPE_REPRESENTATION(#320,#25456);
#486=CONTEXT_DEPENDENT_SHAPE_REPRESENTATION(#321,#25457);
#487=CONTEXT_DEPENDENT_SHAPE_REPRESENTATION(#322,#25458);
#488=CONTEXT_DEPENDENT_SHAPE_REPRESENTATION(#323,#25459);
#489=CONTEXT_DEPENDENT_SHAPE_REPRESENTATION(#324,#25460);
#490=CONTEXT_DEPENDENT_SHAPE_REPRESENTATION(#325,#25461);
#491=CONTEXT_DEPENDENT_SHAPE_REPRESENTATION(#326,#25462);
#492=CONTEXT_DEPENDENT_SHAPE_REPRESENTATION(#327,#25463);
#493=CONTEXT_DEPENDENT_SHAPE_REPRESENTATION(#328,#25464);
#494=CONTEXT_DEPENDENT_SHAPE_REPRESENTATION(#329,#25465);
#495=CONTEXT_DEPENDENT_SHAPE_REPRESENTATION(#330,#25466);
#496=CONTEXT_DEPENDENT_SHAPE_REPRESENTATION(#331,#25467);
#497=CONTEXT_DEPENDENT_SHAPE_REPRESENTATION(#332,#25468);
#498=CONTEXT_DEPENDENT_SHAPE_REPRESENTATION(#333,#25469);
#499=CONTEXT_DEPENDENT_SHAPE_REPRESENTATION(#334,#25470);
#500=CONTEXT_DEPENDENT_SHAPE_REPRESENTATION(#335,#25471);
#501=CONTEXT_DEPENDENT_SHAPE_REPRESENTATION(#336,#25472);
#502=CONTEXT_DEPENDENT_SHAPE_REPRESENTATION(#337,#25473);
#503=CONTEXT_DEPENDENT_SHAPE_REPRESENTATION(#338,#25474);
#504=CONTEXT_DEPENDENT_SHAPE_REPRESENTATION(#339,#25475);
#505=CONTEXT_DEPENDENT_SHAPE_REPRESENTATION(#340,#25476);
#506=CONTEXT_DEPENDENT_SHAPE_REPRESENTATION(#341,#25477);
#507=CONTEXT_DEPENDENT_SHAPE_REPRESENTATION(#342,#25478);
#508=CONTEXT_DEPENDENT_SHAPE_REPRESENTATION(#343,#25479);
#509=CONTEXT_DEPENDENT_SHAPE_REPRESENTATION(#344,#25480);
#510=CONTEXT_DEPENDENT_SHAPE_REPRESENTATION(#345,#25481);
#511=CONTEXT_DEPENDENT_SHAPE_REPRESENTATION(#346,#25482);
#512=CONTEXT_DEPENDENT_SHAPE_REPRESENTATION(#347,#25483);
#513=CONTEXT_DEPENDENT_SHAPE_REPRESENTATION(#348,#25484);
#514=CONTEXT_DEPENDENT_SHAPE_REPRESENTATION(#349,#25485);
#515=CONTEXT_DEPENDENT_SHAPE_REPRESENTATION(#350,#25486);
#516=CONTEXT_DEPENDENT_SHAPE_REPRESENTATION(#351,#25487);
#517=CONTEXT_DEPENDENT_SHAPE_REPRESENTATION(#352,#25488);
#518=CONTEXT_DEPENDENT_SHAPE_REPRESENTATION(#353,#25489);
#519=CONTEXT_DEPENDENT_SHAPE_REPRESENTATION(#354,#25497);
#520=CONTEXT_DEPENDENT_SHAPE_REPRESENTATION(#355,#25498);
#521=CONTEXT_DEPENDENT_SHAPE_REPRESENTATION(#356,#25499);
#522=CONTEXT_DEPENDENT_SHAPE_REPRESENTATION(#357,#25500);
#523=CONTEXT_DEPENDENT_SHAPE_REPRESENTATION(#358,#25501);
#524=CONTEXT_DEPENDENT_SHAPE_REPRESENTATION(#359,#25502);
#525=CONTEXT_DEPENDENT_SHAPE_REPRESENTATION(#360,#25503);
#526=CONTEXT_DEPENDENT_SHAPE_REPRESENTATION(#361,#25504);
#527=CONTEXT_DEPENDENT_SHAPE_REPRESENTATION(#362,#25505);
#528=CONTEXT_DEPENDENT_SHAPE_REPRESENTATION(#363,#25506);
#529=CONTEXT_DEPENDENT_SHAPE_REPRESENTATION(#364,#25507);
#530=CONTEXT_DEPENDENT_SHAPE_REPRESENTATION(#365,#25508);
#531=CONTEXT_DEPENDENT_SHAPE_REPRESENTATION(#366,#25509);
#532=NEXT_ASSEMBLY_USAGE_OCCURRENCE('Steel sleeve:1','Steel sleeve:1',
'Steel sleeve:1',#25689,#25690,'Steel sleeve:1');
#533=NEXT_ASSEMBLY_USAGE_OCCURRENCE('Ball retainer (plastic):1',
'Ball retainer (plastic):1','Ball retainer (plastic):1',#25689,#25691,
'Ball retainer (plastic):1');
#534=NEXT_ASSEMBLY_USAGE_OCCURRENCE('Top plate:1','Top plate:1',
'Top plate:1',#25651,#25652,'Top plate:1');
#535=NEXT_ASSEMBLY_USAGE_OCCURRENCE('Upper fixed end support:1',
'Upper fixed end support:1','Upper fixed end support:1',#25651,#25653,
'Upper fixed end support:1');
#536=NEXT_ASSEMBLY_USAGE_OCCURRENCE('Upper sliding end support:1',
'Upper sliding end support:1','Upper sliding end support:1',#25651,#25654,
'Upper sliding end support:1');
#537=NEXT_ASSEMBLY_USAGE_OCCURRENCE('Guide shaft (2):1',
'Guide shaft (2):1','Guide shaft (2):1',#25651,#25655,
'Guide shaft (2):1');
#538=NEXT_ASSEMBLY_USAGE_OCCURRENCE('Guide shaft (3):1',
'Guide shaft (3):1','Guide shaft (3):1',#25651,#25656,
'Guide shaft (3):1');
#539=NEXT_ASSEMBLY_USAGE_OCCURRENCE('Pivot axle 145 mm:1',
'Pivot axle 145 mm:1','Pivot axle 145 mm:1',#25651,#25657,
'Pivot axle 145 mm:1');
#540=NEXT_ASSEMBLY_USAGE_OCCURRENCE('Axle end keeper (2):1',
'Axle end keeper (2):1','Axle end keeper (2):1',#25651,#25658,
'Axle end keeper (2):1');
#541=NEXT_ASSEMBLY_USAGE_OCCURRENCE('Axle end keeper (3):1',
'Axle end keeper (3):1','Axle end keeper (3):1',#25651,#25659,
'Axle end keeper (3):1');
#542=NEXT_ASSEMBLY_USAGE_OCCURRENCE('Axle distance sleeve 5 mm (2):1',
'Axle distance sleeve 5 mm (2):1','Axle distance sleeve 5 mm (2):1',#25651,
#25660,'Axle distance sleeve 5 mm (2):1');
#543=NEXT_ASSEMBLY_USAGE_OCCURRENCE('Axle distance sleeve 5 mm (3):1',
'Axle distance sleeve 5 mm (3):1','Axle distance sleeve 5 mm (3):1',#25651,
#25661,'Axle distance sleeve 5 mm (3):1');
#544=NEXT_ASSEMBLY_USAGE_OCCURRENCE('Axle distance sleeve 30 mm:1',
'Axle distance sleeve 30 mm:1','Axle distance sleeve 30 mm:1',#25651,#25662,
'Axle distance sleeve 30 mm:1');
#545=NEXT_ASSEMBLY_USAGE_OCCURRENCE('Axle distance sleeve 5 mm (4):1',
'Axle distance sleeve 5 mm (4):1','Axle distance sleeve 5 mm (4):1',#25651,
#25663,'Axle distance sleeve 5 mm (4):1');
#546=NEXT_ASSEMBLY_USAGE_OCCURRENCE('Cap Screw - M5x20:10',
'Cap Screw - M5x20:10','Cap Screw - M5x20:10',#25651,#25664,
'Cap Screw - M5x20:10');
#547=NEXT_ASSEMBLY_USAGE_OCCURRENCE('Cap Screw - M5x20:11',
'Cap Screw - M5x20:11','Cap Screw - M5x20:11',#25651,#25664,
'Cap Screw - M5x20:11');
#548=NEXT_ASSEMBLY_USAGE_OCCURRENCE('Cap Screw - M5x20:12',
'Cap Screw - M5x20:12','Cap Screw - M5x20:12',#25651,#25664,
'Cap Screw - M5x20:12');
#549=NEXT_ASSEMBLY_USAGE_OCCURRENCE('Cap Screw - M5x20:13',
'Cap Screw - M5x20:13','Cap Screw - M5x20:13',#25651,#25664,
'Cap Screw - M5x20:13');
#550=NEXT_ASSEMBLY_USAGE_OCCURRENCE('Cap Screw - M5x20:14',
'Cap Screw - M5x20:14','Cap Screw - M5x20:14',#25651,#25664,
'Cap Screw - M5x20:14');
#551=NEXT_ASSEMBLY_USAGE_OCCURRENCE('Cap Screw - M5x20:15',
'Cap Screw - M5x20:15','Cap Screw - M5x20:15',#25651,#25664,
'Cap Screw - M5x20:15');
#552=NEXT_ASSEMBLY_USAGE_OCCURRENCE('Cap Screw - M5x20:16',
'Cap Screw - M5x20:16','Cap Screw - M5x20:16',#25651,#25664,
'Cap Screw - M5x20:16');
#553=NEXT_ASSEMBLY_USAGE_OCCURRENCE('Cap Screw - M5x20:17',
'Cap Screw - M5x20:17','Cap Screw - M5x20:17',#25651,#25664,
'Cap Screw - M5x20:17');
#554=NEXT_ASSEMBLY_USAGE_OCCURRENCE('Cap Screw - M4x16:4',
'Cap Screw - M4x16:4','Cap Screw - M4x16:4',#25651,#25710,
'Cap Screw - M4x16:4');
#555=NEXT_ASSEMBLY_USAGE_OCCURRENCE('Cap Screw - M4x16:5',
'Cap Screw - M4x16:5','Cap Screw - M4x16:5',#25651,#25710,
'Cap Screw - M4x16:5');
#556=NEXT_ASSEMBLY_USAGE_OCCURRENCE('Lower nut carriage:1',
'Lower nut carriage:1','Lower nut carriage:1',#25665,#25666,
'Lower nut carriage:1');
#557=NEXT_ASSEMBLY_USAGE_OCCURRENCE('Linear bearing keeper:1',
'Linear bearing keeper:1','Linear bearing keeper:1',#25665,#25667,
'Linear bearing keeper:1');
#558=NEXT_ASSEMBLY_USAGE_OCCURRENCE('Linear bearing keeper (1):1',
'Linear bearing keeper (1):1','Linear bearing keeper (1):1',#25665,#25668,
'Linear bearing keeper (1):1');
#559=NEXT_ASSEMBLY_USAGE_OCCURRENCE('Sliding pivot crosshead:1',
'Sliding pivot crosshead:1','Sliding pivot crosshead:1',#25665,#25669,
'Sliding pivot crosshead:1');
#560=NEXT_ASSEMBLY_USAGE_OCCURRENCE('Pivot axle 145 mm (1):1',
'Pivot axle 145 mm (1):1','Pivot axle 145 mm (1):1',#25665,#25670,
'Pivot axle 145 mm (1):1');
#561=NEXT_ASSEMBLY_USAGE_OCCURRENCE('Axle end keeper (4):1',
'Axle end keeper (4):1','Axle end keeper (4):1',#25665,#25671,
'Axle end keeper (4):1');
#562=NEXT_ASSEMBLY_USAGE_OCCURRENCE('Axle end keeper (5):1',
'Axle end keeper (5):1','Axle end keeper (5):1',#25665,#25672,
'Axle end keeper (5):1');
#563=NEXT_ASSEMBLY_USAGE_OCCURRENCE('Axle distance sleeve 5 mm (5):1',
'Axle distance sleeve 5 mm (5):1','Axle distance sleeve 5 mm (5):1',#25665,
#25673,'Axle distance sleeve 5 mm (5):1');
#564=NEXT_ASSEMBLY_USAGE_OCCURRENCE('Axle distance sleeve 10 mm (1):1',
'Axle distance sleeve 10 mm (1):1','Axle distance sleeve 10 mm (1):1',#25665,
#25674,'Axle distance sleeve 10 mm (1):1');
#565=NEXT_ASSEMBLY_USAGE_OCCURRENCE('Axle distance sleeve 35 mm:1',
'Axle distance sleeve 35 mm:1','Axle distance sleeve 35 mm:1',#25665,#25675,
'Axle distance sleeve 35 mm:1');
#566=NEXT_ASSEMBLY_USAGE_OCCURRENCE('Axle distance sleeve 5 mm (6):1',
'Axle distance sleeve 5 mm (6):1','Axle distance sleeve 5 mm (6):1',#25665,
#25676,'Axle distance sleeve 5 mm (6):1');
#567=NEXT_ASSEMBLY_USAGE_OCCURRENCE(
'Linear Ball Bushing - 12 x 21 x 30 mm:2',
'Linear Ball Bushing - 12 x 21 x 30 mm:2',
'Linear Ball Bushing - 12 x 21 x 30 mm:2',#25665,#25689,
'Linear Ball Bushing - 12 x 21 x 30 mm:2');
#568=NEXT_ASSEMBLY_USAGE_OCCURRENCE(
'Linear Ball Bushing - 12 x 21 x 30 mm:3',
'Linear Ball Bushing - 12 x 21 x 30 mm:3',
'Linear Ball Bushing - 12 x 21 x 30 mm:3',#25665,#25689,
'Linear Ball Bushing - 12 x 21 x 30 mm:3');
#569=NEXT_ASSEMBLY_USAGE_OCCURRENCE('M4x4 collar screw:2',
'M4x4 collar screw:2','M4x4 collar screw:2',#25665,#25692,
'M4x4 collar screw:2');
#570=NEXT_ASSEMBLY_USAGE_OCCURRENCE('Cap Screw - M4x16:6',
'Cap Screw - M4x16:6','Cap Screw - M4x16:6',#25665,#25710,
'Cap Screw - M4x16:6');
#571=NEXT_ASSEMBLY_USAGE_OCCURRENCE('Cap Screw - M4x16:7',
'Cap Screw - M4x16:7','Cap Screw - M4x16:7',#25665,#25710,
'Cap Screw - M4x16:7');
#572=NEXT_ASSEMBLY_USAGE_OCCURRENCE('Upper sliding carriage:1',
'Upper sliding carriage:1','Upper sliding carriage:1',#25677,#25678,
'Upper sliding carriage:1');
#573=NEXT_ASSEMBLY_USAGE_OCCURRENCE('Linear bearing keeper (2):1',
'Linear bearing keeper (2):1','Linear bearing keeper (2):1',#25677,#25679,
'Linear bearing keeper (2):1');
#574=NEXT_ASSEMBLY_USAGE_OCCURRENCE('Linear bearing keeper (3):1',
'Linear bearing keeper (3):1','Linear bearing keeper (3):1',#25677,#25680,
'Linear bearing keeper (3):1');
#575=NEXT_ASSEMBLY_USAGE_OCCURRENCE('Sliding pivot crosshead (1):1',
'Sliding pivot crosshead (1):1','Sliding pivot crosshead (1):1',#25677,
#25681,'Sliding pivot crosshead (1):1');
#576=NEXT_ASSEMBLY_USAGE_OCCURRENCE('Pivot axle 140 mm (1):1',
'Pivot axle 140 mm (1):1','Pivot axle 140 mm (1):1',#25677,#25682,
'Pivot axle 140 mm (1):1');
#577=NEXT_ASSEMBLY_USAGE_OCCURRENCE('Axle end keeper (6):1',
'Axle end keeper (6):1','Axle end keeper (6):1',#25677,#25683,
'Axle end keeper (6):1');
#578=NEXT_ASSEMBLY_USAGE_OCCURRENCE('Axle end keeper (7):1',
'Axle end keeper (7):1','Axle end keeper (7):1',#25677,#25684,
'Axle end keeper (7):1');
#579=NEXT_ASSEMBLY_USAGE_OCCURRENCE('Axle distance sleeve 5 mm (7):1',
'Axle distance sleeve 5 mm (7):1','Axle distance sleeve 5 mm (7):1',#25677,
#25685,'Axle distance sleeve 5 mm (7):1');
#580=NEXT_ASSEMBLY_USAGE_OCCURRENCE('Axle distance sleeve 25 mm:1',
'Axle distance sleeve 25 mm:1','Axle distance sleeve 25 mm:1',#25677,#25686,
'Axle distance sleeve 25 mm:1');
#581=NEXT_ASSEMBLY_USAGE_OCCURRENCE('Axle distance sleeve 15 mm:1',
'Axle distance sleeve 15 mm:1','Axle distance sleeve 15 mm:1',#25677,#25687,
'Axle distance sleeve 15 mm:1');
#582=NEXT_ASSEMBLY_USAGE_OCCURRENCE('Axle distance sleeve 5 mm (8):1',
'Axle distance sleeve 5 mm (8):1','Axle distance sleeve 5 mm (8):1',#25677,
#25688,'Axle distance sleeve 5 mm (8):1');
#583=NEXT_ASSEMBLY_USAGE_OCCURRENCE(
'Linear Ball Bushing - 12 x 21 x 30 mm:4',
'Linear Ball Bushing - 12 x 21 x 30 mm:4',
'Linear Ball Bushing - 12 x 21 x 30 mm:4',#25677,#25689,
'Linear Ball Bushing - 12 x 21 x 30 mm:4');
#584=NEXT_ASSEMBLY_USAGE_OCCURRENCE(
'Linear Ball Bushing - 12 x 21 x 30 mm:5',
'Linear Ball Bushing - 12 x 21 x 30 mm:5',
'Linear Ball Bushing - 12 x 21 x 30 mm:5',#25677,#25689,
'Linear Ball Bushing - 12 x 21 x 30 mm:5');
#585=NEXT_ASSEMBLY_USAGE_OCCURRENCE('M4x4 collar screw:3',
'M4x4 collar screw:3','M4x4 collar screw:3',#25677,#25692,
'M4x4 collar screw:3');
#586=NEXT_ASSEMBLY_USAGE_OCCURRENCE('Cap Screw - M4x16:8',
'Cap Screw - M4x16:8','Cap Screw - M4x16:8',#25677,#25710,
'Cap Screw - M4x16:8');
#587=NEXT_ASSEMBLY_USAGE_OCCURRENCE('Cap Screw - M4x16:9',
'Cap Screw - M4x16:9','Cap Screw - M4x16:9',#25677,#25710,
'Cap Screw - M4x16:9');
#588=NEXT_ASSEMBLY_USAGE_OCCURRENCE('Rising arm:1','Rising arm:1',
'Rising arm:1',#25693,#25694,'Rising arm:1');
#589=NEXT_ASSEMBLY_USAGE_OCCURRENCE('Plain pivot bush:1',
'Plain pivot bush:1','Plain pivot bush:1',#25693,#25695,
'Plain pivot bush:1');
#590=NEXT_ASSEMBLY_USAGE_OCCURRENCE('Plain pivot bush (1):1',
'Plain pivot bush (1):1','Plain pivot bush (1):1',#25693,#25696,
'Plain pivot bush (1):1');
#591=NEXT_ASSEMBLY_USAGE_OCCURRENCE('Plain pivot bush (2):1',
'Plain pivot bush (2):1','Plain pivot bush (2):1',#25693,#25697,
'Plain pivot bush (2):1');
#592=NEXT_ASSEMBLY_USAGE_OCCURRENCE('Rising arm (1):1',
'Rising arm (1):1','Rising arm (1):1',#25693,#25698,'Rising arm (1):1');
#593=NEXT_ASSEMBLY_USAGE_OCCURRENCE('Plain pivot bush (3):1',
'Plain pivot bush (3):1','Plain pivot bush (3):1',#25693,#25699,
'Plain pivot bush (3):1');
#594=NEXT_ASSEMBLY_USAGE_OCCURRENCE('Plain pivot bush (4):1',
'Plain pivot bush (4):1','Plain pivot bush (4):1',#25693,#25700,
'Plain pivot bush (4):1');
#595=NEXT_ASSEMBLY_USAGE_OCCURRENCE('Plain pivot bush (5):1',
'Plain pivot bush (5):1','Plain pivot bush (5):1',#25693,#25701,
'Plain pivot bush (5):1');
#596=NEXT_ASSEMBLY_USAGE_OCCURRENCE('Pivot axle 160 mm:1',
'Pivot axle 160 mm:1','Pivot axle 160 mm:1',#25693,#25702,
'Pivot axle 160 mm:1');
#597=NEXT_ASSEMBLY_USAGE_OCCURRENCE('Axle end keeper (8):1',
'Axle end keeper (8):1','Axle end keeper (8):1',#25693,#25703,
'Axle end keeper (8):1');
#598=NEXT_ASSEMBLY_USAGE_OCCURRENCE('Axle end keeper (9):1',
'Axle end keeper (9):1','Axle end keeper (9):1',#25693,#25704,
'Axle end keeper (9):1');
#599=NEXT_ASSEMBLY_USAGE_OCCURRENCE('Axle distance sleeve 5 mm (9):1',
'Axle distance sleeve 5 mm (9):1','Axle distance sleeve 5 mm (9):1',#25693,
#25705,'Axle distance sleeve 5 mm (9):1');
#600=NEXT_ASSEMBLY_USAGE_OCCURRENCE('Axle distance sleeve 5 mm (10):1',
'Axle distance sleeve 5 mm (10):1','Axle distance sleeve 5 mm (10):1',#25693,
#25706,'Axle distance sleeve 5 mm (10):1');
#601=NEXT_ASSEMBLY_USAGE_OCCURRENCE('Axle distance sleeve 95 mm:1',
'Axle distance sleeve 95 mm:1','Axle distance sleeve 95 mm:1',#25693,#25707,
'Axle distance sleeve 95 mm:1');
#602=NEXT_ASSEMBLY_USAGE_OCCURRENCE('Axle distance sleeve 10 mm (2):1',
'Axle distance sleeve 10 mm (2):1','Axle distance sleeve 10 mm (2):1',#25693,
#25708,'Axle distance sleeve 10 mm (2):1');
#603=NEXT_ASSEMBLY_USAGE_OCCURRENCE('Axle distance sleeve 5 mm (11):1',
'Axle distance sleeve 5 mm (11):1','Axle distance sleeve 5 mm (11):1',#25693,
#25709,'Axle distance sleeve 5 mm (11):1');
#604=NEXT_ASSEMBLY_USAGE_OCCURRENCE('Cap Screw - M4x16:10',
'Cap Screw - M4x16:10','Cap Screw - M4x16:10',#25693,#25710,
'Cap Screw - M4x16:10');
#605=NEXT_ASSEMBLY_USAGE_OCCURRENCE('Cap Screw - M4x16:11',
'Cap Screw - M4x16:11','Cap Screw - M4x16:11',#25693,#25710,
'Cap Screw - M4x16:11');
#606=NEXT_ASSEMBLY_USAGE_OCCURRENCE('Inner ring:1','Inner ring:1',
'Inner ring:1',#25738,#25739,'Inner ring:1');
#607=NEXT_ASSEMBLY_USAGE_OCCURRENCE('Outer ring:1','Outer ring:1',
'Outer ring:1',#25738,#25740,'Outer ring:1');
#608=NEXT_ASSEMBLY_USAGE_OCCURRENCE('Balls:1','Balls:1','Balls:1',#25738,
#25741,'Balls:1');
#609=NEXT_ASSEMBLY_USAGE_OCCURRENCE('Cage:1','Cage:1','Cage:1',#25738,#25742,
'Cage:1');
#610=NEXT_ASSEMBLY_USAGE_OCCURRENCE('Seals 2RS:1','Seals 2RS:1',
'Seals 2RS:1',#25738,#25743,'Seals 2RS:1');
#611=NEXT_ASSEMBLY_USAGE_OCCURRENCE('Base plate:1','Base plate:1',
'Base plate:1',#25632,#25633,'Base plate:1');
#612=NEXT_ASSEMBLY_USAGE_OCCURRENCE('Base foot:1','Base foot:1',
'Base foot:1',#25632,#25634,'Base foot:1');
#613=NEXT_ASSEMBLY_USAGE_OCCURRENCE('Base foot (1):1','Base foot (1):1',
'Base foot (1):1',#25632,#25635,'Base foot (1):1');
#614=NEXT_ASSEMBLY_USAGE_OCCURRENCE('Lower pivot support:1',
'Lower pivot support:1','Lower pivot support:1',#25632,#25636,
'Lower pivot support:1');
#615=NEXT_ASSEMBLY_USAGE_OCCURRENCE('Screw bearing cap:1',
'Screw bearing cap:1','Screw bearing cap:1',#25632,#25637,
'Screw bearing cap:1');
#616=NEXT_ASSEMBLY_USAGE_OCCURRENCE('Screw bearing cap (1):1',
'Screw bearing cap (1):1','Screw bearing cap (1):1',#25632,#25638,
'Screw bearing cap (1):1');
#617=NEXT_ASSEMBLY_USAGE_OCCURRENCE('Lower screw support:1',
'Lower screw support:1','Lower screw support:1',#25632,#25639,
'Lower screw support:1');
#618=NEXT_ASSEMBLY_USAGE_OCCURRENCE('Screw bearing cap (2):1',
'Screw bearing cap (2):1','Screw bearing cap (2):1',#25632,#25640,
'Screw bearing cap (2):1');
#619=NEXT_ASSEMBLY_USAGE_OCCURRENCE('Screw bearing cap (3):1',
'Screw bearing cap (3):1','Screw bearing cap (3):1',#25632,#25641,
'Screw bearing cap (3):1');
#620=NEXT_ASSEMBLY_USAGE_OCCURRENCE('Guide shaft:1','Guide shaft:1',
'Guide shaft:1',#25632,#25642,'Guide shaft:1');
#621=NEXT_ASSEMBLY_USAGE_OCCURRENCE('Guide shaft (1):1',
'Guide shaft (1):1','Guide shaft (1):1',#25632,#25643,
'Guide shaft (1):1');
#622=NEXT_ASSEMBLY_USAGE_OCCURRENCE('Pivot axle 140 mm:1',
'Pivot axle 140 mm:1','Pivot axle 140 mm:1',#25632,#25644,
'Pivot axle 140 mm:1');
#623=NEXT_ASSEMBLY_USAGE_OCCURRENCE('Axle end keeper:1',
'Axle end keeper:1','Axle end keeper:1',#25632,#25645,
'Axle end keeper:1');
#624=NEXT_ASSEMBLY_USAGE_OCCURRENCE('Axle end keeper (1):1',
'Axle end keeper (1):1','Axle end keeper (1):1',#25632,#25646,
'Axle end keeper (1):1');
#625=NEXT_ASSEMBLY_USAGE_OCCURRENCE('Axle distance sleeve 5 mm:1',
'Axle distance sleeve 5 mm:1','Axle distance sleeve 5 mm:1',#25632,#25647,
'Axle distance sleeve 5 mm:1');
#626=NEXT_ASSEMBLY_USAGE_OCCURRENCE('Axle distance sleeve 10 mm:1',
'Axle distance sleeve 10 mm:1','Axle distance sleeve 10 mm:1',#25632,#25648,
'Axle distance sleeve 10 mm:1');
#627=NEXT_ASSEMBLY_USAGE_OCCURRENCE('Axle distance sleeve 5 mm (1):1',
'Axle distance sleeve 5 mm (1):1','Axle distance sleeve 5 mm (1):1',#25632,
#25649,'Axle distance sleeve 5 mm (1):1');
#628=NEXT_ASSEMBLY_USAGE_OCCURRENCE('Cap Screw - M5x20:2',
'Cap Screw - M5x20:2','Cap Screw - M5x20:2',#25632,#25664,
'Cap Screw - M5x20:2');
#629=NEXT_ASSEMBLY_USAGE_OCCURRENCE('Cap Screw - M5x20:3',
'Cap Screw - M5x20:3','Cap Screw - M5x20:3',#25632,#25664,
'Cap Screw - M5x20:3');
#630=NEXT_ASSEMBLY_USAGE_OCCURRENCE('Cap Screw - M5x20:4',
'Cap Screw - M5x20:4','Cap Screw - M5x20:4',#25632,#25664,
'Cap Screw - M5x20:4');
#631=NEXT_ASSEMBLY_USAGE_OCCURRENCE('Cap Screw - M5x20:5',
'Cap Screw - M5x20:5','Cap Screw - M5x20:5',#25632,#25664,
'Cap Screw - M5x20:5');
#632=NEXT_ASSEMBLY_USAGE_OCCURRENCE(
'Sealed Ball Bearing - 12 x 32 x 10 mm:2',
'Sealed Ball Bearing - 12 x 32 x 10 mm:2',
'Sealed Ball Bearing - 12 x 32 x 10 mm:2',#25632,#25738,
'Sealed Ball Bearing - 12 x 32 x 10 mm:2');
#633=NEXT_ASSEMBLY_USAGE_OCCURRENCE('M4x10 Cap Screw:2',
'M4x10 Cap Screw:2','M4x10 Cap Screw:2',#25632,#25650,
'M4x10 Cap Screw:2');
#634=NEXT_ASSEMBLY_USAGE_OCCURRENCE('M4x10 Cap Screw:3',
'M4x10 Cap Screw:3','M4x10 Cap Screw:3',#25632,#25650,
'M4x10 Cap Screw:3');
#635=NEXT_ASSEMBLY_USAGE_OCCURRENCE('M4x10 Cap Screw:4',
'M4x10 Cap Screw:4','M4x10 Cap Screw:4',#25632,#25650,
'M4x10 Cap Screw:4');
#636=NEXT_ASSEMBLY_USAGE_OCCURRENCE('M4x10 Cap Screw:5',
'M4x10 Cap Screw:5','M4x10 Cap Screw:5',#25632,#25650,
'M4x10 Cap Screw:5');
#637=NEXT_ASSEMBLY_USAGE_OCCURRENCE('M4x10 Cap Screw:6',
'M4x10 Cap Screw:6','M4x10 Cap Screw:6',#25632,#25650,
'M4x10 Cap Screw:6');
#638=NEXT_ASSEMBLY_USAGE_OCCURRENCE('M4x10 Cap Screw:7',
'M4x10 Cap Screw:7','M4x10 Cap Screw:7',#25632,#25650,
'M4x10 Cap Screw:7');
#639=NEXT_ASSEMBLY_USAGE_OCCURRENCE('M4x10 Cap Screw:8',
'M4x10 Cap Screw:8','M4x10 Cap Screw:8',#25632,#25650,
'M4x10 Cap Screw:8');
#640=NEXT_ASSEMBLY_USAGE_OCCURRENCE('M4x10 Cap Screw:9',
'M4x10 Cap Screw:9','M4x10 Cap Screw:9',#25632,#25650,
'M4x10 Cap Screw:9');
#641=NEXT_ASSEMBLY_USAGE_OCCURRENCE('Cap Screw - M5x20:6',
'Cap Screw - M5x20:6','Cap Screw - M5x20:6',#25632,#25664,
'Cap Screw - M5x20:6');
#642=NEXT_ASSEMBLY_USAGE_OCCURRENCE('Cap Screw - M5x20:7',
'Cap Screw - M5x20:7','Cap Screw - M5x20:7',#25632,#25664,
'Cap Screw - M5x20:7');
#643=NEXT_ASSEMBLY_USAGE_OCCURRENCE('Cap Screw - M5x20:8',
'Cap Screw - M5x20:8','Cap Screw - M5x20:8',#25632,#25664,
'Cap Screw - M5x20:8');
#644=NEXT_ASSEMBLY_USAGE_OCCURRENCE('Cap Screw - M5x20:9',
'Cap Screw - M5x20:9','Cap Screw - M5x20:9',#25632,#25664,
'Cap Screw - M5x20:9');
#645=NEXT_ASSEMBLY_USAGE_OCCURRENCE(
'Sealed Ball Bearing - 12 x 32 x 10 mm:3',
'Sealed Ball Bearing - 12 x 32 x 10 mm:3',
'Sealed Ball Bearing - 12 x 32 x 10 mm:3',#25632,#25738,
'Sealed Ball Bearing - 12 x 32 x 10 mm:3');
#646=NEXT_ASSEMBLY_USAGE_OCCURRENCE('M4x10 Cap Screw:10',
'M4x10 Cap Screw:10','M4x10 Cap Screw:10',#25632,#25650,
'M4x10 Cap Screw:10');
#647=NEXT_ASSEMBLY_USAGE_OCCURRENCE('M4x10 Cap Screw:11',
'M4x10 Cap Screw:11','M4x10 Cap Screw:11',#25632,#25650,
'M4x10 Cap Screw:11');
#648=NEXT_ASSEMBLY_USAGE_OCCURRENCE('M4x10 Cap Screw:12',
'M4x10 Cap Screw:12','M4x10 Cap Screw:12',#25632,#25650,
'M4x10 Cap Screw:12');
#649=NEXT_ASSEMBLY_USAGE_OCCURRENCE('M4x10 Cap Screw:13',
'M4x10 Cap Screw:13','M4x10 Cap Screw:13',#25632,#25650,
'M4x10 Cap Screw:13');
#650=NEXT_ASSEMBLY_USAGE_OCCURRENCE('M4x10 Cap Screw:14',
'M4x10 Cap Screw:14','M4x10 Cap Screw:14',#25632,#25650,
'M4x10 Cap Screw:14');
#651=NEXT_ASSEMBLY_USAGE_OCCURRENCE('M4x10 Cap Screw:15',
'M4x10 Cap Screw:15','M4x10 Cap Screw:15',#25632,#25650,
'M4x10 Cap Screw:15');
#652=NEXT_ASSEMBLY_USAGE_OCCURRENCE('M4x10 Cap Screw:16',
'M4x10 Cap Screw:16','M4x10 Cap Screw:16',#25632,#25650,
'M4x10 Cap Screw:16');
#653=NEXT_ASSEMBLY_USAGE_OCCURRENCE('M4x10 Cap Screw:17',
'M4x10 Cap Screw:17','M4x10 Cap Screw:17',#25632,#25650,
'M4x10 Cap Screw:17');
#654=NEXT_ASSEMBLY_USAGE_OCCURRENCE('Cap Screw - M4x16:2',
'Cap Screw - M4x16:2','Cap Screw - M4x16:2',#25632,#25710,
'Cap Screw - M4x16:2');
#655=NEXT_ASSEMBLY_USAGE_OCCURRENCE('Cap Screw - M4x16:3',
'Cap Screw - M4x16:3','Cap Screw - M4x16:3',#25632,#25710,
'Cap Screw - M4x16:3');
#656=NEXT_ASSEMBLY_USAGE_OCCURRENCE('Crossing arm:1','Crossing arm:1',
'Crossing arm:1',#25711,#25712,'Crossing arm:1');
#657=NEXT_ASSEMBLY_USAGE_OCCURRENCE('Plain pivot bush (6):1',
'Plain pivot bush (6):1','Plain pivot bush (6):1',#25711,#25713,
'Plain pivot bush (6):1');
#658=NEXT_ASSEMBLY_USAGE_OCCURRENCE('Plain pivot bush (7):1',
'Plain pivot bush (7):1','Plain pivot bush (7):1',#25711,#25714,
'Plain pivot bush (7):1');
#659=NEXT_ASSEMBLY_USAGE_OCCURRENCE('Centre bearing retainer:1',
'Centre bearing retainer:1','Centre bearing retainer:1',#25711,#25715,
'Centre bearing retainer:1');
#660=NEXT_ASSEMBLY_USAGE_OCCURRENCE('M4 low-profile retaining screw:1',
'M4 low-profile retaining screw:1','M4 low-profile retaining screw:1',#25711,
#25716,'M4 low-profile retaining screw:1');
#661=NEXT_ASSEMBLY_USAGE_OCCURRENCE(
'M4 low-profile retaining screw (1):1',
'M4 low-profile retaining screw (1):1',
'M4 low-profile retaining screw (1):1',#25711,#25717,
'M4 low-profile retaining screw (1):1');
#662=NEXT_ASSEMBLY_USAGE_OCCURRENCE(
'M4 low-profile retaining screw (2):1',
'M4 low-profile retaining screw (2):1',
'M4 low-profile retaining screw (2):1',#25711,#25718,
'M4 low-profile retaining screw (2):1');
#663=NEXT_ASSEMBLY_USAGE_OCCURRENCE(
'M4 low-profile retaining screw (3):1',
'M4 low-profile retaining screw (3):1',
'M4 low-profile retaining screw (3):1',#25711,#25719,
'M4 low-profile retaining screw (3):1');
#664=NEXT_ASSEMBLY_USAGE_OCCURRENCE('Centre bearing retainer (1):1',
'Centre bearing retainer (1):1','Centre bearing retainer (1):1',#25711,
#25720,'Centre bearing retainer (1):1');
#665=NEXT_ASSEMBLY_USAGE_OCCURRENCE(
'M4 low-profile retaining screw (4):1',
'M4 low-profile retaining screw (4):1',
'M4 low-profile retaining screw (4):1',#25711,#25721,
'M4 low-profile retaining screw (4):1');
#666=NEXT_ASSEMBLY_USAGE_OCCURRENCE(
'M4 low-profile retaining screw (5):1',
'M4 low-profile retaining screw (5):1',
'M4 low-profile retaining screw (5):1',#25711,#25722,
'M4 low-profile retaining screw (5):1');
#667=NEXT_ASSEMBLY_USAGE_OCCURRENCE(
'M4 low-profile retaining screw (6):1',
'M4 low-profile retaining screw (6):1',
'M4 low-profile retaining screw (6):1',#25711,#25723,
'M4 low-profile retaining screw (6):1');
#668=NEXT_ASSEMBLY_USAGE_OCCURRENCE(
'M4 low-profile retaining screw (7):1',
'M4 low-profile retaining screw (7):1',
'M4 low-profile retaining screw (7):1',#25711,#25724,
'M4 low-profile retaining screw (7):1');
#669=NEXT_ASSEMBLY_USAGE_OCCURRENCE('Crossing arm (1):1',
'Crossing arm (1):1','Crossing arm (1):1',#25711,#25725,
'Crossing arm (1):1');
#670=NEXT_ASSEMBLY_USAGE_OCCURRENCE('Plain pivot bush (8):1',
'Plain pivot bush (8):1','Plain pivot bush (8):1',#25711,#25726,
'Plain pivot bush (8):1');
#671=NEXT_ASSEMBLY_USAGE_OCCURRENCE('Plain pivot bush (9):1',
'Plain pivot bush (9):1','Plain pivot bush (9):1',#25711,#25727,
'Plain pivot bush (9):1');
#672=NEXT_ASSEMBLY_USAGE_OCCURRENCE('Centre bearing retainer (2):1',
'Centre bearing retainer (2):1','Centre bearing retainer (2):1',#25711,
#25728,'Centre bearing retainer (2):1');
#673=NEXT_ASSEMBLY_USAGE_OCCURRENCE(
'M4 low-profile retaining screw (8):1',
'M4 low-profile retaining screw (8):1',
'M4 low-profile retaining screw (8):1',#25711,#25729,
'M4 low-profile retaining screw (8):1');
#674=NEXT_ASSEMBLY_USAGE_OCCURRENCE(
'M4 low-profile retaining screw (9):1',
'M4 low-profile retaining screw (9):1',
'M4 low-profile retaining screw (9):1',#25711,#25730,
'M4 low-profile retaining screw (9):1');
#675=NEXT_ASSEMBLY_USAGE_OCCURRENCE(
'M4 low-profile retaining screw (10):1',
'M4 low-profile retaining screw (10):1',
'M4 low-profile retaining screw (10):1',#25711,#25731,
'M4 low-profile retaining screw (10):1');
#676=NEXT_ASSEMBLY_USAGE_OCCURRENCE(
'M4 low-profile retaining screw (11):1',
'M4 low-profile retaining screw (11):1',
'M4 low-profile retaining screw (11):1',#25711,#25732,
'M4 low-profile retaining screw (11):1');
#677=NEXT_ASSEMBLY_USAGE_OCCURRENCE('Centre bearing retainer (3):1',
'Centre bearing retainer (3):1','Centre bearing retainer (3):1',#25711,
#25733,'Centre bearing retainer (3):1');
#678=NEXT_ASSEMBLY_USAGE_OCCURRENCE(
'M4 low-profile retaining screw (12):1',
'M4 low-profile retaining screw (12):1',
'M4 low-profile retaining screw (12):1',#25711,#25734,
'M4 low-profile retaining screw (12):1');
#679=NEXT_ASSEMBLY_USAGE_OCCURRENCE(
'M4 low-profile retaining screw (13):1',
'M4 low-profile retaining screw (13):1',
'M4 low-profile retaining screw (13):1',#25711,#25735,
'M4 low-profile retaining screw (13):1');
#680=NEXT_ASSEMBLY_USAGE_OCCURRENCE(
'M4 low-profile retaining screw (14):1',
'M4 low-profile retaining screw (14):1',
'M4 low-profile retaining screw (14):1',#25711,#25736,
'M4 low-profile retaining screw (14):1');
#681=NEXT_ASSEMBLY_USAGE_OCCURRENCE(
'M4 low-profile retaining screw (15):1',
'M4 low-profile retaining screw (15):1',
'M4 low-profile retaining screw (15):1',#25711,#25737,
'M4 low-profile retaining screw (15):1');
#682=NEXT_ASSEMBLY_USAGE_OCCURRENCE(
'Sealed Ball Bearing - 12 x 32 x 10 mm:4',
'Sealed Ball Bearing - 12 x 32 x 10 mm:4',
'Sealed Ball Bearing - 12 x 32 x 10 mm:4',#25711,#25738,
'Sealed Ball Bearing - 12 x 32 x 10 mm:4');
#683=NEXT_ASSEMBLY_USAGE_OCCURRENCE(
'Sealed Ball Bearing - 12 x 32 x 10 mm:5',
'Sealed Ball Bearing - 12 x 32 x 10 mm:5',
'Sealed Ball Bearing - 12 x 32 x 10 mm:5',#25711,#25738,
'Sealed Ball Bearing - 12 x 32 x 10 mm:5');
#684=NEXT_ASSEMBLY_USAGE_OCCURRENCE('Lead screw:1','Lead screw:1',
'Lead screw:1',#25744,#25745,'Lead screw:1');
#685=NEXT_ASSEMBLY_USAGE_OCCURRENCE('Bearing inner spacer:1',
'Bearing inner spacer:1','Bearing inner spacer:1',#25744,#25746,
'Bearing inner spacer:1');
#686=NEXT_ASSEMBLY_USAGE_OCCURRENCE('Bearing inner spacer (1):1',
'Bearing inner spacer (1):1','Bearing inner spacer (1):1',#25744,#25747,
'Bearing inner spacer (1):1');
#687=NEXT_ASSEMBLY_USAGE_OCCURRENCE('Screw retaining collar:1',
'Screw retaining collar:1','Screw retaining collar:1',#25744,#25748,
'Screw retaining collar:1');
#688=NEXT_ASSEMBLY_USAGE_OCCURRENCE('Screw retaining collar (1):1',
'Screw retaining collar (1):1','Screw retaining collar (1):1',#25744,#25749,
'Screw retaining collar (1):1');
#689=NEXT_ASSEMBLY_USAGE_OCCURRENCE('Handwheel:1','Handwheel:1',
'Handwheel:1',#25744,#25750,'Handwheel:1');
#690=NEXT_ASSEMBLY_USAGE_OCCURRENCE('Base and lower guides:1',
'Base and lower guides:1','Base and lower guides:1',#25631,#25632,
'Base and lower guides:1');
#691=NEXT_ASSEMBLY_USAGE_OCCURRENCE('Top and upper guides:1',
'Top and upper guides:1','Top and upper guides:1',#25631,#25651,
'Top and upper guides:1');
#692=NEXT_ASSEMBLY_USAGE_OCCURRENCE('Lower sliding pivot:1',
'Lower sliding pivot:1','Lower sliding pivot:1',#25631,#25665,
'Lower sliding pivot:1');
#693=NEXT_ASSEMBLY_USAGE_OCCURRENCE('Upper sliding pivot:1',
'Upper sliding pivot:1','Upper sliding pivot:1',#25631,#25677,
'Upper sliding pivot:1');
#694=NEXT_ASSEMBLY_USAGE_OCCURRENCE('Rising arms:1','Rising arms:1',
'Rising arms:1',#25631,#25693,'Rising arms:1');
#695=NEXT_ASSEMBLY_USAGE_OCCURRENCE('Crossing arms:1','Crossing arms:1',
'Crossing arms:1',#25631,#25711,'Crossing arms:1');
#696=NEXT_ASSEMBLY_USAGE_OCCURRENCE('Lead screw and handwheel:1',
'Lead screw and handwheel:1','Lead screw and handwheel:1',#25631,#25744,
'Lead screw and handwheel:1');
#697=B_SPLINE_CURVE_WITH_KNOTS('',3,(#22341,#22342,#22343,#22344,#22345,
#22346,#22347,#22348,#22349,#22350,#22351,#22352,#22353,#22354),
 .UNSPECIFIED.,.F.,.F.,(4,2,2,2,2,2,4),(0.598759558597954,0.624973342427791,
0.687463163426143,0.749952984424496,0.812442805422848,0.874932626421201,
0.901146410251039),.UNSPECIFIED.);
#698=B_SPLINE_CURVE_WITH_KNOTS('',3,(#22362,#22363,#22364,#22365,#22366,
#22367,#22368,#22369,#22370,#22371,#22372,#22373,#22374,#22375),
 .UNSPECIFIED.,.F.,.F.,(4,2,2,2,2,2,4),(0.0987909023149563,0.125004686144793,
0.187494507143146,0.249984328141499,0.312474149139851,0.374963970138204,
0.401177753968041),.UNSPECIFIED.);
#699=B_SPLINE_CURVE_WITH_KNOTS('',3,(#22695,#22696,#22697,#22698,#22699,
#22700,#22701,#22702,#22703,#22704,#22705,#22706,#22707,#22708),
 .UNSPECIFIED.,.F.,.F.,(4,2,2,2,2,2,4),(0.598759558597949,0.624973342427788,
0.68746316342614,0.749952984424493,0.812442805422846,0.874932626421198,
0.901146410251035),.UNSPECIFIED.);
#700=B_SPLINE_CURVE_WITH_KNOTS('',3,(#22716,#22717,#22718,#22719,#22720,
#22721,#22722,#22723,#22724,#22725,#22726,#22727,#22728,#22729),
 .UNSPECIFIED.,.F.,.F.,(4,2,2,2,2,2,4),(0.0987909023149571,0.125004686144792,
0.187494507143145,0.249984328141498,0.31247414913985,0.374963970138203,
0.401177753968041),.UNSPECIFIED.);
#701=B_SPLINE_CURVE_WITH_KNOTS('',3,(#24299,#24300,#24301,#24302,#24303,
#24304),.UNSPECIFIED.,.F.,.F.,(4,2,4),(0.899240844561108,0.954818878854282,
0.98574345825674),.UNSPECIFIED.);
#702=B_SPLINE_CURVE_WITH_KNOTS('',3,(#24308,#24309,#24310,#24311,#24312,
#24313),.UNSPECIFIED.,.F.,.F.,(4,2,4),(1.23862523261148,1.28156721462942,
1.33421556357425),.UNSPECIFIED.);
#703=B_SPLINE_CURVE_WITH_KNOTS('',3,(#24324,#24325,#24326,#24327,#24328,
#24329),.UNSPECIFIED.,.F.,.F.,(4,2,4),(0.959827414101938,1.01247576304677,
1.05541774506471),.UNSPECIFIED.);
#704=B_SPLINE_CURVE_WITH_KNOTS('',3,(#24335,#24336,#24337,#24338,#24339,
#24340),.UNSPECIFIED.,.F.,.F.,(4,2,4),(1.13866312806976,1.16958770747221,
1.22516574176539),.UNSPECIFIED.);
#705=B_SPLINE_CURVE_WITH_KNOTS('',3,(#24347,#24348,#24349,#24350,#24351,
#24352),.UNSPECIFIED.,.F.,.F.,(4,2,4),(0.899240844561108,0.954818878854283,
0.985743458256741),.UNSPECIFIED.);
#706=B_SPLINE_CURVE_WITH_KNOTS('',3,(#24355,#24356,#24357,#24358,#24359,
#24360),.UNSPECIFIED.,.F.,.F.,(4,2,4),(1.23862523261148,1.28156721462942,
1.33421556357425),.UNSPECIFIED.);
#707=B_SPLINE_CURVE_WITH_KNOTS('',3,(#24369,#24370,#24371,#24372,#24373,
#24374),.UNSPECIFIED.,.F.,.F.,(4,2,4),(0.959827414101939,1.01247576304677,
1.05541774506471),.UNSPECIFIED.);
#708=B_SPLINE_CURVE_WITH_KNOTS('',3,(#24379,#24380,#24381,#24382,#24383,
#24384),.UNSPECIFIED.,.F.,.F.,(4,2,4),(1.13866312806975,1.16958770747221,
1.22516574176539),.UNSPECIFIED.);
#709=B_SPLINE_CURVE_WITH_KNOTS('',3,(#24391,#24392,#24393,#24394,#24395,
#24396),.UNSPECIFIED.,.F.,.F.,(4,2,4),(0.899240844561107,0.954818878854282,
0.98574345825674),.UNSPECIFIED.);
#710=B_SPLINE_CURVE_WITH_KNOTS('',3,(#24400,#24401,#24402,#24403,#24404,
#24405),.UNSPECIFIED.,.F.,.F.,(4,2,4),(1.23862523261148,1.28156721462942,
1.33421556357425),.UNSPECIFIED.);
#711=B_SPLINE_CURVE_WITH_KNOTS('',3,(#24411,#24412,#24413,#24414,#24415,
#24416),.UNSPECIFIED.,.F.,.F.,(4,2,4),(0.959827414101938,1.01247576304677,
1.05541774506471),.UNSPECIFIED.);
#712=B_SPLINE_CURVE_WITH_KNOTS('',3,(#24427,#24428,#24429,#24430,#24431,
#24432),.UNSPECIFIED.,.F.,.F.,(4,2,4),(1.13866312806976,1.16958770747221,
1.22516574176539),.UNSPECIFIED.);
#713=B_SPLINE_CURVE_WITH_KNOTS('',3,(#24439,#24440,#24441,#24442,#24443,
#24444),.UNSPECIFIED.,.F.,.F.,(4,2,4),(1.13866312806976,1.16958770747221,
1.22516574176539),.UNSPECIFIED.);
#714=B_SPLINE_CURVE_WITH_KNOTS('',3,(#24447,#24448,#24449,#24450,#24451,
#24452),.UNSPECIFIED.,.F.,.F.,(4,2,4),(0.959827414101938,1.01247576304677,
1.05541774506471),.UNSPECIFIED.);
#715=B_SPLINE_CURVE_WITH_KNOTS('',3,(#24457,#24458,#24459,#24460,#24461,
#24462),.UNSPECIFIED.,.F.,.F.,(4,2,4),(1.23862523261148,1.28156721462942,
1.33421556357425),.UNSPECIFIED.);
#716=B_SPLINE_CURVE_WITH_KNOTS('',3,(#24471,#24472,#24473,#24474,#24475,
#24476),.UNSPECIFIED.,.F.,.F.,(4,2,4),(0.899240844561108,0.954818878854282,
0.985743458256741),.UNSPECIFIED.);
#717=B_SPLINE_CURVE_WITH_KNOTS('',3,(#24483,#24484,#24485,#24486,#24487,
#24488),.UNSPECIFIED.,.F.,.F.,(4,2,4),(1.13866312806975,1.16958770747221,
1.22516574176539),.UNSPECIFIED.);
#718=B_SPLINE_CURVE_WITH_KNOTS('',3,(#24492,#24493,#24494,#24495,#24496,
#24497),.UNSPECIFIED.,.F.,.F.,(4,2,4),(0.959827414101939,1.01247576304677,
1.05541774506471),.UNSPECIFIED.);
#719=B_SPLINE_CURVE_WITH_KNOTS('',3,(#24502,#24503,#24504,#24505,#24506,
#24507),.UNSPECIFIED.,.F.,.F.,(4,2,4),(0.899240844561108,0.954818878854282,
0.985743458256741),.UNSPECIFIED.);
#720=B_SPLINE_CURVE_WITH_KNOTS('',3,(#24519,#24520,#24521,#24522,#24523,
#24524),.UNSPECIFIED.,.F.,.F.,(4,2,4),(1.23862523261148,1.28156721462942,
1.33421556357425),.UNSPECIFIED.);
#721=B_SPLINE_CURVE_WITH_KNOTS('',3,(#24529,#24530,#24531,#24532,#24533,
#24534),.UNSPECIFIED.,.F.,.F.,(4,2,4),(1.13866312806976,1.16958770747221,
1.22516574176539),.UNSPECIFIED.);
#722=B_SPLINE_CURVE_WITH_KNOTS('',3,(#24538,#24539,#24540,#24541,#24542,
#24543),.UNSPECIFIED.,.F.,.F.,(4,2,4),(0.959827414101938,1.01247576304677,
1.05541774506471),.UNSPECIFIED.);
#723=B_SPLINE_CURVE_WITH_KNOTS('',3,(#24548,#24549,#24550,#24551,#24552,
#24553),.UNSPECIFIED.,.F.,.F.,(4,2,4),(0.899240844561108,0.954818878854282,
0.98574345825674),.UNSPECIFIED.);
#724=B_SPLINE_CURVE_WITH_KNOTS('',3,(#24562,#24563,#24564,#24565,#24566,
#24567),.UNSPECIFIED.,.F.,.F.,(4,2,4),(1.23862523261148,1.28156721462942,
1.33421556357425),.UNSPECIFIED.);
#725=B_SPLINE_CURVE_WITH_KNOTS('',3,(#24575,#24576,#24577,#24578,#24579,
#24580),.UNSPECIFIED.,.F.,.F.,(4,2,4),(1.23862523261148,1.28156721462942,
1.33421556357425),.UNSPECIFIED.);
#726=B_SPLINE_CURVE_WITH_KNOTS('',3,(#24584,#24585,#24586,#24587,#24588,
#24589),.UNSPECIFIED.,.F.,.F.,(4,2,4),(0.959827414101938,1.01247576304677,
1.05541774506471),.UNSPECIFIED.);
#727=B_SPLINE_CURVE_WITH_KNOTS('',3,(#24600,#24601,#24602,#24603,#24604,
#24605),.UNSPECIFIED.,.F.,.F.,(4,2,4),(1.13866312806976,1.16958770747221,
1.22516574176539),.UNSPECIFIED.);
#728=B_SPLINE_CURVE_WITH_KNOTS('',3,(#24611,#24612,#24613,#24614,#24615,
#24616),.UNSPECIFIED.,.F.,.F.,(4,2,4),(0.899240844561108,0.954818878854282,
0.98574345825674),.UNSPECIFIED.);
#729=CONICAL_SURFACE('',#14907,0.325,0.785398163397448);
#730=CONICAL_SURFACE('',#14911,0.335,0.785398163397448);
#731=CONICAL_SURFACE('',#14915,0.21,0.463647609000806);
#732=CONICAL_SURFACE('',#15095,0.4,0.785398163397448);
#733=CONICAL_SURFACE('',#15099,0.41,0.785398163397448);
#734=CONICAL_SURFACE('',#15103,0.26,0.463647609000806);
#735=CONICAL_SURFACE('',#15107,0.225,0.785398163397448);
#736=CONICAL_SURFACE('',#15482,0.185,0.785398163397449);
#737=CONICAL_SURFACE('',#15676,0.325,0.785398163397448);
#738=CONICAL_SURFACE('',#15680,0.335,0.785398163397448);
#739=CONICAL_SURFACE('',#15684,0.21,0.463647609000806);
#740=CONICAL_SURFACE('',#15688,0.18,0.785398163397448);
#741=CONICAL_SURFACE('',#16145,0.63,0.785398163397448);
#742=CONICAL_SURFACE('',#16152,0.63,0.785398163397448);
#743=CONICAL_SURFACE('',#16165,1.57,0.785398163397449);
#744=CONICAL_SURFACE('',#16169,1.57,0.785398163397449);
#745=ORIENTED_CLOSED_SHELL('',*,#13265,.F.);
#746=ORIENTED_CLOSED_SHELL('',*,#13280,.F.);
#747=ORIENTED_CLOSED_SHELL('',*,#13323,.F.);
#748=BREP_WITH_VOIDS('Body1',#13266,(#745));
#749=BREP_WITH_VOIDS('Body1',#13279,(#746));
#750=BREP_WITH_VOIDS('Body1',#13322,(#747));
#751=SHAPE_REPRESENTATION_RELATIONSHIP('SRR','None',#25512,#861);
#752=SHAPE_REPRESENTATION_RELATIONSHIP('SRR','None',#25513,#862);
#753=SHAPE_REPRESENTATION_RELATIONSHIP('SRR','None',#25514,#863);
#754=SHAPE_REPRESENTATION_RELATIONSHIP('SRR','None',#25515,#864);
#755=SHAPE_REPRESENTATION_RELATIONSHIP('SRR','None',#25516,#865);
#756=SHAPE_REPRESENTATION_RELATIONSHIP('SRR','None',#25517,#866);
#757=SHAPE_REPRESENTATION_RELATIONSHIP('SRR','None',#25518,#867);
#758=SHAPE_REPRESENTATION_RELATIONSHIP('SRR','None',#25519,#868);
#759=SHAPE_REPRESENTATION_RELATIONSHIP('SRR','None',#25520,#869);
#760=SHAPE_REPRESENTATION_RELATIONSHIP('SRR','None',#25521,#870);
#761=SHAPE_REPRESENTATION_RELATIONSHIP('SRR','None',#25522,#871);
#762=SHAPE_REPRESENTATION_RELATIONSHIP('SRR','None',#25523,#872);
#763=SHAPE_REPRESENTATION_RELATIONSHIP('SRR','None',#25524,#873);
#764=SHAPE_REPRESENTATION_RELATIONSHIP('SRR','None',#25525,#874);
#765=SHAPE_REPRESENTATION_RELATIONSHIP('SRR','None',#25526,#875);
#766=SHAPE_REPRESENTATION_RELATIONSHIP('SRR','None',#25527,#876);
#767=SHAPE_REPRESENTATION_RELATIONSHIP('SRR','None',#25528,#877);
#768=SHAPE_REPRESENTATION_RELATIONSHIP('SRR','None',#25529,#878);
#769=SHAPE_REPRESENTATION_RELATIONSHIP('SRR','None',#25531,#879);
#770=SHAPE_REPRESENTATION_RELATIONSHIP('SRR','None',#25532,#880);
#771=SHAPE_REPRESENTATION_RELATIONSHIP('SRR','None',#25533,#881);
#772=SHAPE_REPRESENTATION_RELATIONSHIP('SRR','None',#25534,#882);
#773=SHAPE_REPRESENTATION_RELATIONSHIP('SRR','None',#25535,#883);
#774=SHAPE_REPRESENTATION_RELATIONSHIP('SRR','None',#25536,#884);
#775=SHAPE_REPRESENTATION_RELATIONSHIP('SRR','None',#25537,#885);
#776=SHAPE_REPRESENTATION_RELATIONSHIP('SRR','None',#25538,#886);
#777=SHAPE_REPRESENTATION_RELATIONSHIP('SRR','None',#25539,#887);
#778=SHAPE_REPRESENTATION_RELATIONSHIP('SRR','None',#25540,#888);
#779=SHAPE_REPRESENTATION_RELATIONSHIP('SRR','None',#25541,#889);
#780=SHAPE_REPRESENTATION_RELATIONSHIP('SRR','None',#25542,#890);
#781=SHAPE_REPRESENTATION_RELATIONSHIP('SRR','None',#25543,#891);
#782=SHAPE_REPRESENTATION_RELATIONSHIP('SRR','None',#25545,#892);
#783=SHAPE_REPRESENTATION_RELATIONSHIP('SRR','None',#25546,#893);
#784=SHAPE_REPRESENTATION_RELATIONSHIP('SRR','None',#25547,#894);
#785=SHAPE_REPRESENTATION_RELATIONSHIP('SRR','None',#25548,#895);
#786=SHAPE_REPRESENTATION_RELATIONSHIP('SRR','None',#25549,#896);
#787=SHAPE_REPRESENTATION_RELATIONSHIP('SRR','None',#25550,#897);
#788=SHAPE_REPRESENTATION_RELATIONSHIP('SRR','None',#25551,#898);
#789=SHAPE_REPRESENTATION_RELATIONSHIP('SRR','None',#25552,#899);
#790=SHAPE_REPRESENTATION_RELATIONSHIP('SRR','None',#25553,#900);
#791=SHAPE_REPRESENTATION_RELATIONSHIP('SRR','None',#25554,#901);
#792=SHAPE_REPRESENTATION_RELATIONSHIP('SRR','None',#25555,#902);
#793=SHAPE_REPRESENTATION_RELATIONSHIP('SRR','None',#25557,#903);
#794=SHAPE_REPRESENTATION_RELATIONSHIP('SRR','None',#25558,#904);
#795=SHAPE_REPRESENTATION_RELATIONSHIP('SRR','None',#25559,#905);
#796=SHAPE_REPRESENTATION_RELATIONSHIP('SRR','None',#25560,#906);
#797=SHAPE_REPRESENTATION_RELATIONSHIP('SRR','None',#25561,#907);
#798=SHAPE_REPRESENTATION_RELATIONSHIP('SRR','None',#25562,#908);
#799=SHAPE_REPRESENTATION_RELATIONSHIP('SRR','None',#25563,#909);
#800=SHAPE_REPRESENTATION_RELATIONSHIP('SRR','None',#25564,#910);
#801=SHAPE_REPRESENTATION_RELATIONSHIP('SRR','None',#25565,#911);
#802=SHAPE_REPRESENTATION_RELATIONSHIP('SRR','None',#25566,#912);
#803=SHAPE_REPRESENTATION_RELATIONSHIP('SRR','None',#25567,#913);
#804=SHAPE_REPRESENTATION_RELATIONSHIP('SRR','None',#25569,#914);
#805=SHAPE_REPRESENTATION_RELATIONSHIP('SRR','None',#25570,#915);
#806=SHAPE_REPRESENTATION_RELATIONSHIP('SRR','None',#25571,#916);
#807=SHAPE_REPRESENTATION_RELATIONSHIP('SRR','None',#25573,#917);
#808=SHAPE_REPRESENTATION_RELATIONSHIP('SRR','None',#25574,#918);
#809=SHAPE_REPRESENTATION_RELATIONSHIP('SRR','None',#25575,#919);
#810=SHAPE_REPRESENTATION_RELATIONSHIP('SRR','None',#25576,#920);
#811=SHAPE_REPRESENTATION_RELATIONSHIP('SRR','None',#25577,#921);
#812=SHAPE_REPRESENTATION_RELATIONSHIP('SRR','None',#25578,#922);
#813=SHAPE_REPRESENTATION_RELATIONSHIP('SRR','None',#25579,#923);
#814=SHAPE_REPRESENTATION_RELATIONSHIP('SRR','None',#25580,#924);
#815=SHAPE_REPRESENTATION_RELATIONSHIP('SRR','None',#25581,#925);
#816=SHAPE_REPRESENTATION_RELATIONSHIP('SRR','None',#25582,#926);
#817=SHAPE_REPRESENTATION_RELATIONSHIP('SRR','None',#25583,#927);
#818=SHAPE_REPRESENTATION_RELATIONSHIP('SRR','None',#25584,#928);
#819=SHAPE_REPRESENTATION_RELATIONSHIP('SRR','None',#25585,#929);
#820=SHAPE_REPRESENTATION_RELATIONSHIP('SRR','None',#25586,#930);
#821=SHAPE_REPRESENTATION_RELATIONSHIP('SRR','None',#25587,#931);
#822=SHAPE_REPRESENTATION_RELATIONSHIP('SRR','None',#25588,#932);
#823=SHAPE_REPRESENTATION_RELATIONSHIP('SRR','None',#25589,#933);
#824=SHAPE_REPRESENTATION_RELATIONSHIP('SRR','None',#25591,#934);
#825=SHAPE_REPRESENTATION_RELATIONSHIP('SRR','None',#25592,#935);
#826=SHAPE_REPRESENTATION_RELATIONSHIP('SRR','None',#25593,#936);
#827=SHAPE_REPRESENTATION_RELATIONSHIP('SRR','None',#25594,#937);
#828=SHAPE_REPRESENTATION_RELATIONSHIP('SRR','None',#25595,#938);
#829=SHAPE_REPRESENTATION_RELATIONSHIP('SRR','None',#25596,#939);
#830=SHAPE_REPRESENTATION_RELATIONSHIP('SRR','None',#25597,#940);
#831=SHAPE_REPRESENTATION_RELATIONSHIP('SRR','None',#25598,#941);
#832=SHAPE_REPRESENTATION_RELATIONSHIP('SRR','None',#25599,#942);
#833=SHAPE_REPRESENTATION_RELATIONSHIP('SRR','None',#25600,#943);
#834=SHAPE_REPRESENTATION_RELATIONSHIP('SRR','None',#25601,#944);
#835=SHAPE_REPRESENTATION_RELATIONSHIP('SRR','None',#25602,#945);
#836=SHAPE_REPRESENTATION_RELATIONSHIP('SRR','None',#25603,#946);
#837=SHAPE_REPRESENTATION_RELATIONSHIP('SRR','None',#25604,#947);
#838=SHAPE_REPRESENTATION_RELATIONSHIP('SRR','None',#25605,#948);
#839=SHAPE_REPRESENTATION_RELATIONSHIP('SRR','None',#25606,#949);
#840=SHAPE_REPRESENTATION_RELATIONSHIP('SRR','None',#25607,#950);
#841=SHAPE_REPRESENTATION_RELATIONSHIP('SRR','None',#25608,#951);
#842=SHAPE_REPRESENTATION_RELATIONSHIP('SRR','None',#25609,#952);
#843=SHAPE_REPRESENTATION_RELATIONSHIP('SRR','None',#25610,#953);
#844=SHAPE_REPRESENTATION_RELATIONSHIP('SRR','None',#25611,#954);
#845=SHAPE_REPRESENTATION_RELATIONSHIP('SRR','None',#25612,#955);
#846=SHAPE_REPRESENTATION_RELATIONSHIP('SRR','None',#25613,#956);
#847=SHAPE_REPRESENTATION_RELATIONSHIP('SRR','None',#25614,#957);
#848=SHAPE_REPRESENTATION_RELATIONSHIP('SRR','None',#25615,#958);
#849=SHAPE_REPRESENTATION_RELATIONSHIP('SRR','None',#25616,#959);
#850=SHAPE_REPRESENTATION_RELATIONSHIP('SRR','None',#25618,#960);
#851=SHAPE_REPRESENTATION_RELATIONSHIP('SRR','None',#25619,#961);
#852=SHAPE_REPRESENTATION_RELATIONSHIP('SRR','None',#25620,#962);
#853=SHAPE_REPRESENTATION_RELATIONSHIP('SRR','None',#25621,#963);
#854=SHAPE_REPRESENTATION_RELATIONSHIP('SRR','None',#25622,#964);
#855=SHAPE_REPRESENTATION_RELATIONSHIP('SRR','None',#25624,#965);
#856=SHAPE_REPRESENTATION_RELATIONSHIP('SRR','None',#25625,#966);
#857=SHAPE_REPRESENTATION_RELATIONSHIP('SRR','None',#25626,#967);
#858=SHAPE_REPRESENTATION_RELATIONSHIP('SRR','None',#25627,#968);
#859=SHAPE_REPRESENTATION_RELATIONSHIP('SRR','None',#25628,#969);
#860=SHAPE_REPRESENTATION_RELATIONSHIP('SRR','None',#25629,#970);
#861=ADVANCED_BREP_SHAPE_REPRESENTATION('',(#1095),#24982);
#862=ADVANCED_BREP_SHAPE_REPRESENTATION('',(#1096),#24983);
#863=ADVANCED_BREP_SHAPE_REPRESENTATION('',(#1097),#24984);
#864=ADVANCED_BREP_SHAPE_REPRESENTATION('',(#1098),#24985);
#865=ADVANCED_BREP_SHAPE_REPRESENTATION('',(#1099),#24986);
#866=ADVANCED_BREP_SHAPE_REPRESENTATION('',(#1100),#24987);
#867=ADVANCED_BREP_SHAPE_REPRESENTATION('',(#1101),#24988);
#868=ADVANCED_BREP_SHAPE_REPRESENTATION('',(#1102),#24989);
#869=ADVANCED_BREP_SHAPE_REPRESENTATION('',(#1103),#24990);
#870=ADVANCED_BREP_SHAPE_REPRESENTATION('',(#1104),#24991);
#871=ADVANCED_BREP_SHAPE_REPRESENTATION('',(#1105),#24992);
#872=ADVANCED_BREP_SHAPE_REPRESENTATION('',(#1106),#24993);
#873=ADVANCED_BREP_SHAPE_REPRESENTATION('',(#1107),#24994);
#874=ADVANCED_BREP_SHAPE_REPRESENTATION('',(#1108),#24995);
#875=ADVANCED_BREP_SHAPE_REPRESENTATION('',(#1109),#24996);
#876=ADVANCED_BREP_SHAPE_REPRESENTATION('',(#1110),#24997);
#877=ADVANCED_BREP_SHAPE_REPRESENTATION('',(#1111),#24998);
#878=ADVANCED_BREP_SHAPE_REPRESENTATION('',(#748),#24999);
#879=ADVANCED_BREP_SHAPE_REPRESENTATION('',(#1112),#25001);
#880=ADVANCED_BREP_SHAPE_REPRESENTATION('',(#1113),#25002);
#881=ADVANCED_BREP_SHAPE_REPRESENTATION('',(#1114),#25003);
#882=ADVANCED_BREP_SHAPE_REPRESENTATION('',(#1115),#25004);
#883=ADVANCED_BREP_SHAPE_REPRESENTATION('',(#1116),#25005);
#884=ADVANCED_BREP_SHAPE_REPRESENTATION('',(#1117),#25006);
#885=ADVANCED_BREP_SHAPE_REPRESENTATION('',(#1118),#25007);
#886=ADVANCED_BREP_SHAPE_REPRESENTATION('',(#1119),#25008);
#887=ADVANCED_BREP_SHAPE_REPRESENTATION('',(#1120),#25009);
#888=ADVANCED_BREP_SHAPE_REPRESENTATION('',(#1121),#25010);
#889=ADVANCED_BREP_SHAPE_REPRESENTATION('',(#1122),#25011);
#890=ADVANCED_BREP_SHAPE_REPRESENTATION('',(#1123),#25012);
#891=ADVANCED_BREP_SHAPE_REPRESENTATION('',(#749),#25013);
#892=ADVANCED_BREP_SHAPE_REPRESENTATION('',(#1124),#25015);
#893=ADVANCED_BREP_SHAPE_REPRESENTATION('',(#1125),#25016);
#894=ADVANCED_BREP_SHAPE_REPRESENTATION('',(#1126),#25017);
#895=ADVANCED_BREP_SHAPE_REPRESENTATION('',(#1127),#25018);
#896=ADVANCED_BREP_SHAPE_REPRESENTATION('',(#1128),#25019);
#897=ADVANCED_BREP_SHAPE_REPRESENTATION('',(#1129),#25020);
#898=ADVANCED_BREP_SHAPE_REPRESENTATION('',(#1130),#25021);
#899=ADVANCED_BREP_SHAPE_REPRESENTATION('',(#1131),#25022);
#900=ADVANCED_BREP_SHAPE_REPRESENTATION('',(#1132),#25023);
#901=ADVANCED_BREP_SHAPE_REPRESENTATION('',(#1133),#25024);
#902=ADVANCED_BREP_SHAPE_REPRESENTATION('',(#1134),#25025);
#903=ADVANCED_BREP_SHAPE_REPRESENTATION('',(#1135),#25027);
#904=ADVANCED_BREP_SHAPE_REPRESENTATION('',(#1136),#25028);
#905=ADVANCED_BREP_SHAPE_REPRESENTATION('',(#1137),#25029);
#906=ADVANCED_BREP_SHAPE_REPRESENTATION('',(#1138),#25030);
#907=ADVANCED_BREP_SHAPE_REPRESENTATION('',(#1139),#25031);
#908=ADVANCED_BREP_SHAPE_REPRESENTATION('',(#1140),#25032);
#909=ADVANCED_BREP_SHAPE_REPRESENTATION('',(#1141),#25033);
#910=ADVANCED_BREP_SHAPE_REPRESENTATION('',(#1142),#25034);
#911=ADVANCED_BREP_SHAPE_REPRESENTATION('',(#1143),#25035);
#912=ADVANCED_BREP_SHAPE_REPRESENTATION('',(#1144),#25036);
#913=ADVANCED_BREP_SHAPE_REPRESENTATION('',(#1145),#25037);
#914=ADVANCED_BREP_SHAPE_REPRESENTATION('',(#1146),#25039);
#915=ADVANCED_BREP_SHAPE_REPRESENTATION('',(#1147),#25040);
#916=ADVANCED_BREP_SHAPE_REPRESENTATION('',(#1148),#25041);
#917=ADVANCED_BREP_SHAPE_REPRESENTATION('',(#1149),#25043);
#918=ADVANCED_BREP_SHAPE_REPRESENTATION('',(#1150),#25044);
#919=ADVANCED_BREP_SHAPE_REPRESENTATION('',(#1151),#25045);
#920=ADVANCED_BREP_SHAPE_REPRESENTATION('',(#1152),#25046);
#921=ADVANCED_BREP_SHAPE_REPRESENTATION('',(#1153),#25047);
#922=ADVANCED_BREP_SHAPE_REPRESENTATION('',(#1154),#25048);
#923=ADVANCED_BREP_SHAPE_REPRESENTATION('',(#1155),#25049);
#924=ADVANCED_BREP_SHAPE_REPRESENTATION('',(#1156),#25050);
#925=ADVANCED_BREP_SHAPE_REPRESENTATION('',(#1157),#25051);
#926=ADVANCED_BREP_SHAPE_REPRESENTATION('',(#1158),#25052);
#927=ADVANCED_BREP_SHAPE_REPRESENTATION('',(#1159),#25053);
#928=ADVANCED_BREP_SHAPE_REPRESENTATION('',(#1160),#25054);
#929=ADVANCED_BREP_SHAPE_REPRESENTATION('',(#1161),#25055);
#930=ADVANCED_BREP_SHAPE_REPRESENTATION('',(#1162),#25056);
#931=ADVANCED_BREP_SHAPE_REPRESENTATION('',(#1163),#25057);
#932=ADVANCED_BREP_SHAPE_REPRESENTATION('',(#1164),#25058);
#933=ADVANCED_BREP_SHAPE_REPRESENTATION('',(#750),#25059);
#934=ADVANCED_BREP_SHAPE_REPRESENTATION('',(#1165),#25061);
#935=ADVANCED_BREP_SHAPE_REPRESENTATION('',(#1166),#25062);
#936=ADVANCED_BREP_SHAPE_REPRESENTATION('',(#1167),#25063);
#937=ADVANCED_BREP_SHAPE_REPRESENTATION('',(#1168),#25064);
#938=ADVANCED_BREP_SHAPE_REPRESENTATION('',(#1169),#25065);
#939=ADVANCED_BREP_SHAPE_REPRESENTATION('',(#1170),#25066);
#940=ADVANCED_BREP_SHAPE_REPRESENTATION('',(#1171),#25067);
#941=ADVANCED_BREP_SHAPE_REPRESENTATION('',(#1172),#25068);
#942=ADVANCED_BREP_SHAPE_REPRESENTATION('',(#1173),#25069);
#943=ADVANCED_BREP_SHAPE_REPRESENTATION('',(#1174),#25070);
#944=ADVANCED_BREP_SHAPE_REPRESENTATION('',(#1175),#25071);
#945=ADVANCED_BREP_SHAPE_REPRESENTATION('',(#1176),#25072);
#946=ADVANCED_BREP_SHAPE_REPRESENTATION('',(#1177),#25073);
#947=ADVANCED_BREP_SHAPE_REPRESENTATION('',(#1178),#25074);
#948=ADVANCED_BREP_SHAPE_REPRESENTATION('',(#1179),#25075);
#949=ADVANCED_BREP_SHAPE_REPRESENTATION('',(#1180),#25076);
#950=ADVANCED_BREP_SHAPE_REPRESENTATION('',(#1181),#25077);
#951=ADVANCED_BREP_SHAPE_REPRESENTATION('',(#1182),#25078);
#952=ADVANCED_BREP_SHAPE_REPRESENTATION('',(#1183),#25079);
#953=ADVANCED_BREP_SHAPE_REPRESENTATION('',(#1184),#25080);
#954=ADVANCED_BREP_SHAPE_REPRESENTATION('',(#1185),#25081);
#955=ADVANCED_BREP_SHAPE_REPRESENTATION('',(#1186),#25082);
#956=ADVANCED_BREP_SHAPE_REPRESENTATION('',(#1187),#25083);
#957=ADVANCED_BREP_SHAPE_REPRESENTATION('',(#1188),#25084);
#958=ADVANCED_BREP_SHAPE_REPRESENTATION('',(#1189),#25085);
#959=ADVANCED_BREP_SHAPE_REPRESENTATION('',(#1190),#25086);
#960=ADVANCED_BREP_SHAPE_REPRESENTATION('',(#1191),#25088);
#961=ADVANCED_BREP_SHAPE_REPRESENTATION('',(#1192),#25089);
#962=ADVANCED_BREP_SHAPE_REPRESENTATION('',(#1193,#1194,#1195,#1196,#1197,
#1198,#1199),#25090);
#963=ADVANCED_BREP_SHAPE_REPRESENTATION('',(#1200,#1201,#1202,#1203,#1204,
#1205,#1206),#25091);
#964=ADVANCED_BREP_SHAPE_REPRESENTATION('',(#1207,#1208),#25092);
#965=ADVANCED_BREP_SHAPE_REPRESENTATION('',(#1209),#25094);
#966=ADVANCED_BREP_SHAPE_REPRESENTATION('',(#1210),#25095);
#967=ADVANCED_BREP_SHAPE_REPRESENTATION('',(#1211),#25096);
#968=ADVANCED_BREP_SHAPE_REPRESENTATION('',(#1212),#25097);
#969=ADVANCED_BREP_SHAPE_REPRESENTATION('',(#1213),#25098);
#970=ADVANCED_BREP_SHAPE_REPRESENTATION('',(#1214),#25099);
#971=STYLED_ITEM('',(#26170),#1095);
#972=STYLED_ITEM('',(#26170),#1096);
#973=STYLED_ITEM('',(#26170),#1097);
#974=STYLED_ITEM('',(#26177),#1098);
#975=STYLED_ITEM('',(#26198),#1099);
#976=STYLED_ITEM('',(#26198),#1100);
#977=STYLED_ITEM('',(#26198),#1101);
#978=STYLED_ITEM('',(#26198),#1102);
#979=STYLED_ITEM('',(#26198),#1103);
#980=STYLED_ITEM('',(#26191),#1104);
#981=STYLED_ITEM('',(#26191),#1105);
#982=STYLED_ITEM('',(#26191),#1106);
#983=STYLED_ITEM('',(#26191),#1107);
#984=STYLED_ITEM('',(#26191),#1108);
#985=STYLED_ITEM('',(#26191),#1109);
#986=STYLED_ITEM('',(#26191),#1110);
#987=STYLED_ITEM('',(#26191),#1111);
#988=STYLED_ITEM('',(#26198),#748);
#989=STYLED_ITEM('',(#26177),#1112);
#990=STYLED_ITEM('',(#26184),#1113);
#991=STYLED_ITEM('',(#26184),#1114);
#992=STYLED_ITEM('',(#26191),#1115);
#993=STYLED_ITEM('',(#26191),#1116);
#994=STYLED_ITEM('',(#26191),#1117);
#995=STYLED_ITEM('',(#26191),#1118);
#996=STYLED_ITEM('',(#26191),#1119);
#997=STYLED_ITEM('',(#26191),#1120);
#998=STYLED_ITEM('',(#26191),#1121);
#999=STYLED_ITEM('',(#26191),#1122);
#1000=STYLED_ITEM('',(#26191),#1123);
#1001=STYLED_ITEM('',(#26198),#749);
#1002=STYLED_ITEM('',(#26198),#1124);
#1003=STYLED_ITEM('',(#26191),#1125);
#1004=STYLED_ITEM('',(#26191),#1126);
#1005=STYLED_ITEM('',(#26205),#1127);
#1006=STYLED_ITEM('',(#26191),#1128);
#1007=STYLED_ITEM('',(#26191),#1129);
#1008=STYLED_ITEM('',(#26191),#1130);
#1009=STYLED_ITEM('',(#26191),#1131);
#1010=STYLED_ITEM('',(#26191),#1132);
#1011=STYLED_ITEM('',(#26191),#1133);
#1012=STYLED_ITEM('',(#26191),#1134);
#1013=STYLED_ITEM('',(#26177),#1135);
#1014=STYLED_ITEM('',(#26191),#1136);
#1015=STYLED_ITEM('',(#26191),#1137);
#1016=STYLED_ITEM('',(#26205),#1138);
#1017=STYLED_ITEM('',(#26191),#1139);
#1018=STYLED_ITEM('',(#26191),#1140);
#1019=STYLED_ITEM('',(#26191),#1141);
#1020=STYLED_ITEM('',(#26191),#1142);
#1021=STYLED_ITEM('',(#26191),#1143);
#1022=STYLED_ITEM('',(#26191),#1144);
#1023=STYLED_ITEM('',(#26191),#1145);
#1024=STYLED_ITEM('',(#26205),#1146);
#1025=STYLED_ITEM('',(#26184),#1147);
#1026=STYLED_ITEM('',(#26198),#1148);
#1027=STYLED_ITEM('',(#26177),#1149);
#1028=STYLED_ITEM('',(#26177),#1150);
#1029=STYLED_ITEM('',(#26177),#1151);
#1030=STYLED_ITEM('',(#26177),#1152);
#1031=STYLED_ITEM('',(#26177),#1153);
#1032=STYLED_ITEM('',(#26177),#1154);
#1033=STYLED_ITEM('',(#26177),#1155);
#1034=STYLED_ITEM('',(#26177),#1156);
#1035=STYLED_ITEM('',(#26191),#1157);
#1036=STYLED_ITEM('',(#26191),#1158);
#1037=STYLED_ITEM('',(#26191),#1159);
#1038=STYLED_ITEM('',(#26191),#1160);
#1039=STYLED_ITEM('',(#26191),#1161);
#1040=STYLED_ITEM('',(#26191),#1162);
#1041=STYLED_ITEM('',(#26191),#1163);
#1042=STYLED_ITEM('',(#26191),#1164);
#1043=STYLED_ITEM('',(#26198),#750);
#1044=STYLED_ITEM('',(#26177),#1165);
#1045=STYLED_ITEM('',(#26177),#1166);
#1046=STYLED_ITEM('',(#26177),#1167);
#1047=STYLED_ITEM('',(#26191),#1168);
#1048=STYLED_ITEM('',(#26198),#1169);
#1049=STYLED_ITEM('',(#26198),#1170);
#1050=STYLED_ITEM('',(#26198),#1171);
#1051=STYLED_ITEM('',(#26198),#1172);
#1052=STYLED_ITEM('',(#26191),#1173);
#1053=STYLED_ITEM('',(#26198),#1174);
#1054=STYLED_ITEM('',(#26198),#1175);
#1055=STYLED_ITEM('',(#26198),#1176);
#1056=STYLED_ITEM('',(#26198),#1177);
#1057=STYLED_ITEM('',(#26177),#1178);
#1058=STYLED_ITEM('',(#26177),#1179);
#1059=STYLED_ITEM('',(#26177),#1180);
#1060=STYLED_ITEM('',(#26191),#1181);
#1061=STYLED_ITEM('',(#26198),#1182);
#1062=STYLED_ITEM('',(#26198),#1183);
#1063=STYLED_ITEM('',(#26198),#1184);
#1064=STYLED_ITEM('',(#26198),#1185);
#1065=STYLED_ITEM('',(#26191),#1186);
#1066=STYLED_ITEM('',(#26198),#1187);
#1067=STYLED_ITEM('',(#26198),#1188);
#1068=STYLED_ITEM('',(#26198),#1189);
#1069=STYLED_ITEM('',(#26198),#1190);
#1070=STYLED_ITEM('',(#26191),#1191);
#1071=STYLED_ITEM('',(#26191),#1192);
#1072=STYLED_ITEM('',(#26191),#1193);
#1073=STYLED_ITEM('',(#26191),#1194);
#1074=STYLED_ITEM('',(#26191),#1195);
#1075=STYLED_ITEM('',(#26191),#1196);
#1076=STYLED_ITEM('',(#26191),#1197);
#1077=STYLED_ITEM('',(#26191),#1198);
#1078=STYLED_ITEM('',(#26191),#1199);
#1079=STYLED_ITEM('',(#26191),#1200);
#1080=STYLED_ITEM('',(#26191),#1201);
#1081=STYLED_ITEM('',(#26191),#1202);
#1082=STYLED_ITEM('',(#26191),#1203);
#1083=STYLED_ITEM('',(#26191),#1204);
#1084=STYLED_ITEM('',(#26191),#1205);
#1085=STYLED_ITEM('',(#26191),#1206);
#1086=STYLED_ITEM('',(#26191),#1207);
#1087=STYLED_ITEM('',(#26191),#1208);
#1088=STYLED_ITEM('',(#26198),#1209);
#1089=STYLED_ITEM('',(#26191),#1210);
#1090=STYLED_ITEM('',(#26191),#1211);
#1091=STYLED_ITEM('',(#26198),#1212);
#1092=STYLED_ITEM('',(#26198),#1213);
#1093=STYLED_ITEM('',(#26184),#1214);
#1094=STYLED_ITEM('',(#26121),#12);
#1095=MANIFOLD_SOLID_BREP('Body1',#13248);
#1096=MANIFOLD_SOLID_BREP('Body1',#13249);
#1097=MANIFOLD_SOLID_BREP('Body1',#13250);
#1098=MANIFOLD_SOLID_BREP('Body1',#13251);
#1099=MANIFOLD_SOLID_BREP('Body1',#13252);
#1100=MANIFOLD_SOLID_BREP('Body1',#13253);
#1101=MANIFOLD_SOLID_BREP('Body1',#13254);
#1102=MANIFOLD_SOLID_BREP('Body1',#13255);
#1103=MANIFOLD_SOLID_BREP('Body1',#13256);
#1104=MANIFOLD_SOLID_BREP('Body1',#13257);
#1105=MANIFOLD_SOLID_BREP('Body1',#13258);
#1106=MANIFOLD_SOLID_BREP('Body1',#13259);
#1107=MANIFOLD_SOLID_BREP('Body1',#13260);
#1108=MANIFOLD_SOLID_BREP('Body1',#13261);
#1109=MANIFOLD_SOLID_BREP('Body1',#13262);
#1110=MANIFOLD_SOLID_BREP('Body1',#13263);
#1111=MANIFOLD_SOLID_BREP('Body1',#13264);
#1112=MANIFOLD_SOLID_BREP('Body1',#13267);
#1113=MANIFOLD_SOLID_BREP('Body1',#13268);
#1114=MANIFOLD_SOLID_BREP('Body1',#13269);
#1115=MANIFOLD_SOLID_BREP('Body1',#13270);
#1116=MANIFOLD_SOLID_BREP('Body1',#13271);
#1117=MANIFOLD_SOLID_BREP('Body1',#13272);
#1118=MANIFOLD_SOLID_BREP('Body1',#13273);
#1119=MANIFOLD_SOLID_BREP('Body1',#13274);
#1120=MANIFOLD_SOLID_BREP('Body1',#13275);
#1121=MANIFOLD_SOLID_BREP('Body1',#13276);
#1122=MANIFOLD_SOLID_BREP('Body1',#13277);
#1123=MANIFOLD_SOLID_BREP('Body1',#13278);
#1124=MANIFOLD_SOLID_BREP('Body1',#13281);
#1125=MANIFOLD_SOLID_BREP('Body1',#13282);
#1126=MANIFOLD_SOLID_BREP('Body1',#13283);
#1127=MANIFOLD_SOLID_BREP('Body1',#13284);
#1128=MANIFOLD_SOLID_BREP('Body1',#13285);
#1129=MANIFOLD_SOLID_BREP('Body1',#13286);
#1130=MANIFOLD_SOLID_BREP('Body1',#13287);
#1131=MANIFOLD_SOLID_BREP('Body1',#13288);
#1132=MANIFOLD_SOLID_BREP('Body1',#13289);
#1133=MANIFOLD_SOLID_BREP('Body1',#13290);
#1134=MANIFOLD_SOLID_BREP('Body1',#13291);
#1135=MANIFOLD_SOLID_BREP('Body1',#13292);
#1136=MANIFOLD_SOLID_BREP('Body1',#13293);
#1137=MANIFOLD_SOLID_BREP('Body1',#13294);
#1138=MANIFOLD_SOLID_BREP('Body1',#13295);
#1139=MANIFOLD_SOLID_BREP('Body1',#13296);
#1140=MANIFOLD_SOLID_BREP('Body1',#13297);
#1141=MANIFOLD_SOLID_BREP('Body1',#13298);
#1142=MANIFOLD_SOLID_BREP('Body1',#13299);
#1143=MANIFOLD_SOLID_BREP('Body1',#13300);
#1144=MANIFOLD_SOLID_BREP('Body1',#13301);
#1145=MANIFOLD_SOLID_BREP('Body1',#13302);
#1146=MANIFOLD_SOLID_BREP('Body1',#13303);
#1147=MANIFOLD_SOLID_BREP('Body1',#13304);
#1148=MANIFOLD_SOLID_BREP('Body1',#13305);
#1149=MANIFOLD_SOLID_BREP('Body1',#13306);
#1150=MANIFOLD_SOLID_BREP('Body1',#13307);
#1151=MANIFOLD_SOLID_BREP('Body1',#13308);
#1152=MANIFOLD_SOLID_BREP('Body1',#13309);
#1153=MANIFOLD_SOLID_BREP('Body1',#13310);
#1154=MANIFOLD_SOLID_BREP('Body1',#13311);
#1155=MANIFOLD_SOLID_BREP('Body1',#13312);
#1156=MANIFOLD_SOLID_BREP('Body1',#13313);
#1157=MANIFOLD_SOLID_BREP('Body1',#13314);
#1158=MANIFOLD_SOLID_BREP('Body1',#13315);
#1159=MANIFOLD_SOLID_BREP('Body1',#13316);
#1160=MANIFOLD_SOLID_BREP('Body1',#13317);
#1161=MANIFOLD_SOLID_BREP('Body1',#13318);
#1162=MANIFOLD_SOLID_BREP('Body1',#13319);
#1163=MANIFOLD_SOLID_BREP('Body1',#13320);
#1164=MANIFOLD_SOLID_BREP('Body1',#13321);
#1165=MANIFOLD_SOLID_BREP('Body1',#13324);
#1166=MANIFOLD_SOLID_BREP('Body1',#13325);
#1167=MANIFOLD_SOLID_BREP('Body1',#13326);
#1168=MANIFOLD_SOLID_BREP('Body1',#13327);
#1169=MANIFOLD_SOLID_BREP('Body1',#13328);
#1170=MANIFOLD_SOLID_BREP('Body1',#13329);
#1171=MANIFOLD_SOLID_BREP('Body1',#13330);
#1172=MANIFOLD_SOLID_BREP('Body1',#13331);
#1173=MANIFOLD_SOLID_BREP('Body1',#13332);
#1174=MANIFOLD_SOLID_BREP('Body1',#13333);
#1175=MANIFOLD_SOLID_BREP('Body1',#13334);
#1176=MANIFOLD_SOLID_BREP('Body1',#13335);
#1177=MANIFOLD_SOLID_BREP('Body1',#13336);
#1178=MANIFOLD_SOLID_BREP('Body1',#13337);
#1179=MANIFOLD_SOLID_BREP('Body1',#13338);
#1180=MANIFOLD_SOLID_BREP('Body1',#13339);
#1181=MANIFOLD_SOLID_BREP('Body1',#13340);
#1182=MANIFOLD_SOLID_BREP('Body1',#13341);
#1183=MANIFOLD_SOLID_BREP('Body1',#13342);
#1184=MANIFOLD_SOLID_BREP('Body1',#13343);
#1185=MANIFOLD_SOLID_BREP('Body1',#13344);
#1186=MANIFOLD_SOLID_BREP('Body1',#13345);
#1187=MANIFOLD_SOLID_BREP('Body1',#13346);
#1188=MANIFOLD_SOLID_BREP('Body1',#13347);
#1189=MANIFOLD_SOLID_BREP('Body1',#13348);
#1190=MANIFOLD_SOLID_BREP('Body1',#13349);
#1191=MANIFOLD_SOLID_BREP('Body1',#13350);
#1192=MANIFOLD_SOLID_BREP('Body1',#13351);
#1193=MANIFOLD_SOLID_BREP('Body1',#13352);
#1194=MANIFOLD_SOLID_BREP('Body2',#13353);
#1195=MANIFOLD_SOLID_BREP('Body3',#13354);
#1196=MANIFOLD_SOLID_BREP('Body4',#13355);
#1197=MANIFOLD_SOLID_BREP('Body5',#13356);
#1198=MANIFOLD_SOLID_BREP('Body6',#13357);
#1199=MANIFOLD_SOLID_BREP('Body7',#13358);
#1200=MANIFOLD_SOLID_BREP('Body1',#13359);
#1201=MANIFOLD_SOLID_BREP('Body9',#13360);
#1202=MANIFOLD_SOLID_BREP('Body10',#13361);
#1203=MANIFOLD_SOLID_BREP('Body11',#13362);
#1204=MANIFOLD_SOLID_BREP('Body12',#13363);
#1205=MANIFOLD_SOLID_BREP('Body13',#13364);
#1206=MANIFOLD_SOLID_BREP('Body14',#13365);
#1207=MANIFOLD_SOLID_BREP('Body1',#13366);
#1208=MANIFOLD_SOLID_BREP('Body2',#13367);
#1209=MANIFOLD_SOLID_BREP('Body1',#13368);
#1210=MANIFOLD_SOLID_BREP('Body1',#13369);
#1211=MANIFOLD_SOLID_BREP('Body1',#13370);
#1212=MANIFOLD_SOLID_BREP('Body1',#13371);
#1213=MANIFOLD_SOLID_BREP('Body1',#13372);
#1214=MANIFOLD_SOLID_BREP('Body1',#13373);
#1215=FACE_BOUND('',#2894,.T.);
#1216=FACE_BOUND('',#2895,.T.);
#1217=FACE_BOUND('',#2896,.T.);
#1218=FACE_BOUND('',#2897,.T.);
#1219=FACE_BOUND('',#2898,.T.);
#1220=FACE_BOUND('',#2899,.T.);
#1221=FACE_BOUND('',#2900,.T.);
#1222=FACE_BOUND('',#2901,.T.);
#1223=FACE_BOUND('',#2903,.T.);
#1224=FACE_BOUND('',#2904,.T.);
#1225=FACE_BOUND('',#2905,.T.);
#1226=FACE_BOUND('',#2906,.T.);
#1227=FACE_BOUND('',#2907,.T.);
#1228=FACE_BOUND('',#2908,.T.);
#1229=FACE_BOUND('',#2909,.T.);
#1230=FACE_BOUND('',#2910,.T.);
#1231=FACE_BOUND('',#2933,.T.);
#1232=FACE_BOUND('',#2934,.T.);
#1233=FACE_BOUND('',#2936,.T.);
#1234=FACE_BOUND('',#2937,.T.);
#1235=FACE_BOUND('',#2941,.T.);
#1236=FACE_BOUND('',#2943,.T.);
#1237=FACE_BOUND('',#2944,.T.);
#1238=FACE_BOUND('',#2945,.T.);
#1239=FACE_BOUND('',#2946,.T.);
#1240=FACE_BOUND('',#2947,.T.);
#1241=FACE_BOUND('',#2948,.T.);
#1242=FACE_BOUND('',#2949,.T.);
#1243=FACE_BOUND('',#2954,.T.);
#1244=FACE_BOUND('',#2955,.T.);
#1245=FACE_BOUND('',#2956,.T.);
#1246=FACE_BOUND('',#2957,.T.);
#1247=FACE_BOUND('',#2958,.T.);
#1248=FACE_BOUND('',#2959,.T.);
#1249=FACE_BOUND('',#2960,.T.);
#1250=FACE_BOUND('',#2962,.T.);
#1251=FACE_BOUND('',#2965,.T.);
#1252=FACE_BOUND('',#2966,.T.);
#1253=FACE_BOUND('',#2967,.T.);
#1254=FACE_BOUND('',#2968,.T.);
#1255=FACE_BOUND('',#2975,.T.);
#1256=FACE_BOUND('',#2979,.T.);
#1257=FACE_BOUND('',#2980,.T.);
#1258=FACE_BOUND('',#2981,.T.);
#1259=FACE_BOUND('',#2982,.T.);
#1260=FACE_BOUND('',#2983,.T.);
#1261=FACE_BOUND('',#2985,.T.);
#1262=FACE_BOUND('',#2986,.T.);
#1263=FACE_BOUND('',#2987,.T.);
#1264=FACE_BOUND('',#2988,.T.);
#1265=FACE_BOUND('',#2989,.T.);
#1266=FACE_BOUND('',#2996,.T.);
#1267=FACE_BOUND('',#3000,.T.);
#1268=FACE_BOUND('',#3001,.T.);
#1269=FACE_BOUND('',#3002,.T.);
#1270=FACE_BOUND('',#3003,.T.);
#1271=FACE_BOUND('',#3004,.T.);
#1272=FACE_BOUND('',#3006,.T.);
#1273=FACE_BOUND('',#3007,.T.);
#1274=FACE_BOUND('',#3008,.T.);
#1275=FACE_BOUND('',#3009,.T.);
#1276=FACE_BOUND('',#3010,.T.);
#1277=FACE_BOUND('',#3021,.T.);
#1278=FACE_BOUND('',#3022,.T.);
#1279=FACE_BOUND('',#3024,.T.);
#1280=FACE_BOUND('',#3025,.T.);
#1281=FACE_BOUND('',#3030,.T.);
#1282=FACE_BOUND('',#3031,.T.);
#1283=FACE_BOUND('',#3032,.T.);
#1284=FACE_BOUND('',#3033,.T.);
#1285=FACE_BOUND('',#3034,.T.);
#1286=FACE_BOUND('',#3035,.T.);
#1287=FACE_BOUND('',#3036,.T.);
#1288=FACE_BOUND('',#3040,.T.);
#1289=FACE_BOUND('',#3041,.T.);
#1290=FACE_BOUND('',#3042,.T.);
#1291=FACE_BOUND('',#3043,.T.);
#1292=FACE_BOUND('',#3044,.T.);
#1293=FACE_BOUND('',#3045,.T.);
#1294=FACE_BOUND('',#3046,.T.);
#1295=FACE_BOUND('',#3050,.T.);
#1296=FACE_BOUND('',#3051,.T.);
#1297=FACE_BOUND('',#3052,.T.);
#1298=FACE_BOUND('',#3053,.T.);
#1299=FACE_BOUND('',#3060,.T.);
#1300=FACE_BOUND('',#3064,.T.);
#1301=FACE_BOUND('',#3065,.T.);
#1302=FACE_BOUND('',#3066,.T.);
#1303=FACE_BOUND('',#3067,.T.);
#1304=FACE_BOUND('',#3068,.T.);
#1305=FACE_BOUND('',#3070,.T.);
#1306=FACE_BOUND('',#3071,.T.);
#1307=FACE_BOUND('',#3072,.T.);
#1308=FACE_BOUND('',#3073,.T.);
#1309=FACE_BOUND('',#3074,.T.);
#1310=FACE_BOUND('',#3081,.T.);
#1311=FACE_BOUND('',#3085,.T.);
#1312=FACE_BOUND('',#3086,.T.);
#1313=FACE_BOUND('',#3087,.T.);
#1314=FACE_BOUND('',#3088,.T.);
#1315=FACE_BOUND('',#3089,.T.);
#1316=FACE_BOUND('',#3091,.T.);
#1317=FACE_BOUND('',#3092,.T.);
#1318=FACE_BOUND('',#3093,.T.);
#1319=FACE_BOUND('',#3094,.T.);
#1320=FACE_BOUND('',#3095,.T.);
#1321=FACE_BOUND('',#3108,.T.);
#1322=FACE_BOUND('',#3110,.T.);
#1323=FACE_BOUND('',#3114,.T.);
#1324=FACE_BOUND('',#3116,.T.);
#1325=FACE_BOUND('',#3120,.T.);
#1326=FACE_BOUND('',#3122,.T.);
#1327=FACE_BOUND('',#3126,.T.);
#1328=FACE_BOUND('',#3128,.T.);
#1329=FACE_BOUND('',#3132,.T.);
#1330=FACE_BOUND('',#3134,.T.);
#1331=FACE_BOUND('',#3138,.T.);
#1332=FACE_BOUND('',#3140,.T.);
#1333=FACE_BOUND('',#3155,.T.);
#1334=FACE_BOUND('',#3171,.T.);
#1335=FACE_BOUND('',#3172,.T.);
#1336=FACE_BOUND('',#3173,.T.);
#1337=FACE_BOUND('',#3174,.T.);
#1338=FACE_BOUND('',#3175,.T.);
#1339=FACE_BOUND('',#3176,.T.);
#1340=FACE_BOUND('',#3177,.T.);
#1341=FACE_BOUND('',#3178,.T.);
#1342=FACE_BOUND('',#3180,.T.);
#1343=FACE_BOUND('',#3181,.T.);
#1344=FACE_BOUND('',#3182,.T.);
#1345=FACE_BOUND('',#3183,.T.);
#1346=FACE_BOUND('',#3184,.T.);
#1347=FACE_BOUND('',#3185,.T.);
#1348=FACE_BOUND('',#3186,.T.);
#1349=FACE_BOUND('',#3187,.T.);
#1350=FACE_BOUND('',#3193,.T.);
#1351=FACE_BOUND('',#3194,.T.);
#1352=FACE_BOUND('',#3195,.T.);
#1353=FACE_BOUND('',#3196,.T.);
#1354=FACE_BOUND('',#3197,.T.);
#1355=FACE_BOUND('',#3203,.T.);
#1356=FACE_BOUND('',#3205,.T.);
#1357=FACE_BOUND('',#3206,.T.);
#1358=FACE_BOUND('',#3211,.T.);
#1359=FACE_BOUND('',#3213,.T.);
#1360=FACE_BOUND('',#3214,.T.);
#1361=FACE_BOUND('',#3216,.T.);
#1362=FACE_BOUND('',#3217,.T.);
#1363=FACE_BOUND('',#3218,.T.);
#1364=FACE_BOUND('',#3219,.T.);
#1365=FACE_BOUND('',#3226,.T.);
#1366=FACE_BOUND('',#3227,.T.);
#1367=FACE_BOUND('',#3231,.T.);
#1368=FACE_BOUND('',#3232,.T.);
#1369=FACE_BOUND('',#3234,.T.);
#1370=FACE_BOUND('',#3235,.T.);
#1371=FACE_BOUND('',#3241,.T.);
#1372=FACE_BOUND('',#3242,.T.);
#1373=FACE_BOUND('',#3244,.T.);
#1374=FACE_BOUND('',#3245,.T.);
#1375=FACE_BOUND('',#3246,.T.);
#1376=FACE_BOUND('',#3247,.T.);
#1377=FACE_BOUND('',#3261,.T.);
#1378=FACE_BOUND('',#3263,.T.);
#1379=FACE_BOUND('',#3267,.T.);
#1380=FACE_BOUND('',#3269,.T.);
#1381=FACE_BOUND('',#3273,.T.);
#1382=FACE_BOUND('',#3275,.T.);
#1383=FACE_BOUND('',#3279,.T.);
#1384=FACE_BOUND('',#3281,.T.);
#1385=FACE_BOUND('',#3285,.T.);
#1386=FACE_BOUND('',#3287,.T.);
#1387=FACE_BOUND('',#3291,.T.);
#1388=FACE_BOUND('',#3293,.T.);
#1389=FACE_BOUND('',#3297,.T.);
#1390=FACE_BOUND('',#3299,.T.);
#1391=FACE_BOUND('',#3305,.T.);
#1392=FACE_BOUND('',#3323,.T.);
#1393=FACE_BOUND('',#3324,.T.);
#1394=FACE_BOUND('',#3325,.T.);
#1395=FACE_BOUND('',#3328,.T.);
#1396=FACE_BOUND('',#3329,.T.);
#1397=FACE_BOUND('',#3330,.T.);
#1398=FACE_BOUND('',#3335,.T.);
#1399=FACE_BOUND('',#3338,.T.);
#1400=FACE_BOUND('',#3347,.T.);
#1401=FACE_BOUND('',#3348,.T.);
#1402=FACE_BOUND('',#3349,.T.);
#1403=FACE_BOUND('',#3351,.T.);
#1404=FACE_BOUND('',#3352,.T.);
#1405=FACE_BOUND('',#3353,.T.);
#1406=FACE_BOUND('',#3356,.T.);
#1407=FACE_BOUND('',#3359,.T.);
#1408=FACE_BOUND('',#3368,.T.);
#1409=FACE_BOUND('',#3369,.T.);
#1410=FACE_BOUND('',#3370,.T.);
#1411=FACE_BOUND('',#3372,.T.);
#1412=FACE_BOUND('',#3373,.T.);
#1413=FACE_BOUND('',#3374,.T.);
#1414=FACE_BOUND('',#3379,.T.);
#1415=FACE_BOUND('',#3381,.T.);
#1416=FACE_BOUND('',#3383,.T.);
#1417=FACE_BOUND('',#3385,.T.);
#1418=FACE_BOUND('',#3395,.T.);
#1419=FACE_BOUND('',#3397,.T.);
#1420=FACE_BOUND('',#3401,.T.);
#1421=FACE_BOUND('',#3403,.T.);
#1422=FACE_BOUND('',#3407,.T.);
#1423=FACE_BOUND('',#3409,.T.);
#1424=FACE_BOUND('',#3413,.T.);
#1425=FACE_BOUND('',#3415,.T.);
#1426=FACE_BOUND('',#3419,.T.);
#1427=FACE_BOUND('',#3421,.T.);
#1428=FACE_BOUND('',#3425,.T.);
#1429=FACE_BOUND('',#3427,.T.);
#1430=FACE_BOUND('',#3431,.T.);
#1431=FACE_BOUND('',#3433,.T.);
#1432=FACE_BOUND('',#3439,.T.);
#1433=FACE_BOUND('',#3440,.T.);
#1434=FACE_BOUND('',#3441,.T.);
#1435=FACE_BOUND('',#3444,.T.);
#1436=FACE_BOUND('',#3445,.T.);
#1437=FACE_BOUND('',#3446,.T.);
#1438=FACE_BOUND('',#3451,.T.);
#1439=FACE_BOUND('',#3454,.T.);
#1440=FACE_BOUND('',#3463,.T.);
#1441=FACE_BOUND('',#3464,.T.);
#1442=FACE_BOUND('',#3465,.T.);
#1443=FACE_BOUND('',#3467,.T.);
#1444=FACE_BOUND('',#3468,.T.);
#1445=FACE_BOUND('',#3469,.T.);
#1446=FACE_BOUND('',#3472,.T.);
#1447=FACE_BOUND('',#3475,.T.);
#1448=FACE_BOUND('',#3484,.T.);
#1449=FACE_BOUND('',#3485,.T.);
#1450=FACE_BOUND('',#3486,.T.);
#1451=FACE_BOUND('',#3488,.T.);
#1452=FACE_BOUND('',#3489,.T.);
#1453=FACE_BOUND('',#3490,.T.);
#1454=FACE_BOUND('',#3495,.T.);
#1455=FACE_BOUND('',#3497,.T.);
#1456=FACE_BOUND('',#3499,.T.);
#1457=FACE_BOUND('',#3501,.T.);
#1458=FACE_BOUND('',#3511,.T.);
#1459=FACE_BOUND('',#3513,.T.);
#1460=FACE_BOUND('',#3517,.T.);
#1461=FACE_BOUND('',#3519,.T.);
#1462=FACE_BOUND('',#3523,.T.);
#1463=FACE_BOUND('',#3525,.T.);
#1464=FACE_BOUND('',#3529,.T.);
#1465=FACE_BOUND('',#3531,.T.);
#1466=FACE_BOUND('',#3535,.T.);
#1467=FACE_BOUND('',#3537,.T.);
#1468=FACE_BOUND('',#3541,.T.);
#1469=FACE_BOUND('',#3543,.T.);
#1470=FACE_BOUND('',#3547,.T.);
#1471=FACE_BOUND('',#3549,.T.);
#1472=FACE_BOUND('',#3556,.T.);
#1473=FACE_BOUND('',#3559,.T.);
#1474=FACE_BOUND('',#3562,.T.);
#1475=FACE_BOUND('',#3565,.T.);
#1476=FACE_BOUND('',#3568,.T.);
#1477=FACE_BOUND('',#3571,.T.);
#1478=FACE_BOUND('',#3573,.T.);
#1479=FACE_BOUND('',#3579,.T.);
#1480=FACE_BOUND('',#3581,.T.);
#1481=FACE_BOUND('',#3583,.T.);
#1482=FACE_BOUND('',#3585,.T.);
#1483=FACE_BOUND('',#3595,.T.);
#1484=FACE_BOUND('',#3607,.T.);
#1485=FACE_BOUND('',#3608,.T.);
#1486=FACE_BOUND('',#3609,.T.);
#1487=FACE_BOUND('',#3614,.T.);
#1488=FACE_BOUND('',#3615,.T.);
#1489=FACE_BOUND('',#3616,.T.);
#1490=FACE_BOUND('',#3620,.T.);
#1491=FACE_BOUND('',#3622,.T.);
#1492=FACE_BOUND('',#3626,.T.);
#1493=FACE_BOUND('',#3628,.T.);
#1494=FACE_BOUND('',#3632,.T.);
#1495=FACE_BOUND('',#3634,.T.);
#1496=FACE_BOUND('',#3644,.T.);
#1497=FACE_BOUND('',#3645,.T.);
#1498=FACE_BOUND('',#3646,.T.);
#1499=FACE_BOUND('',#3651,.T.);
#1500=FACE_BOUND('',#3652,.T.);
#1501=FACE_BOUND('',#3653,.T.);
#1502=FACE_BOUND('',#3657,.T.);
#1503=FACE_BOUND('',#3659,.T.);
#1504=FACE_BOUND('',#3663,.T.);
#1505=FACE_BOUND('',#3665,.T.);
#1506=FACE_BOUND('',#3669,.T.);
#1507=FACE_BOUND('',#3671,.T.);
#1508=FACE_BOUND('',#3678,.T.);
#1509=FACE_BOUND('',#3680,.T.);
#1510=FACE_BOUND('',#3684,.T.);
#1511=FACE_BOUND('',#3686,.T.);
#1512=FACE_BOUND('',#3690,.T.);
#1513=FACE_BOUND('',#3692,.T.);
#1514=FACE_BOUND('',#3696,.T.);
#1515=FACE_BOUND('',#3698,.T.);
#1516=FACE_BOUND('',#3702,.T.);
#1517=FACE_BOUND('',#3704,.T.);
#1518=FACE_BOUND('',#3708,.T.);
#1519=FACE_BOUND('',#3710,.T.);
#1520=FACE_BOUND('',#3714,.T.);
#1521=FACE_BOUND('',#3716,.T.);
#1522=FACE_BOUND('',#3720,.T.);
#1523=FACE_BOUND('',#3722,.T.);
#1524=FACE_BOUND('',#3728,.T.);
#1525=FACE_BOUND('',#3750,.T.);
#1526=FACE_BOUND('',#3751,.T.);
#1527=FACE_BOUND('',#3752,.T.);
#1528=FACE_BOUND('',#3753,.T.);
#1529=FACE_BOUND('',#3754,.T.);
#1530=FACE_BOUND('',#3755,.T.);
#1531=FACE_BOUND('',#3756,.T.);
#1532=FACE_BOUND('',#3765,.T.);
#1533=FACE_BOUND('',#3766,.T.);
#1534=FACE_BOUND('',#3767,.T.);
#1535=FACE_BOUND('',#3768,.T.);
#1536=FACE_BOUND('',#3769,.T.);
#1537=FACE_BOUND('',#3770,.T.);
#1538=FACE_BOUND('',#3771,.T.);
#1539=FACE_BOUND('',#3775,.T.);
#1540=FACE_BOUND('',#3777,.T.);
#1541=FACE_BOUND('',#3781,.T.);
#1542=FACE_BOUND('',#3783,.T.);
#1543=FACE_BOUND('',#3791,.T.);
#1544=FACE_BOUND('',#3792,.T.);
#1545=FACE_BOUND('',#3793,.T.);
#1546=FACE_BOUND('',#3794,.T.);
#1547=FACE_BOUND('',#3795,.T.);
#1548=FACE_BOUND('',#3797,.T.);
#1549=FACE_BOUND('',#3798,.T.);
#1550=FACE_BOUND('',#3799,.T.);
#1551=FACE_BOUND('',#3800,.T.);
#1552=FACE_BOUND('',#3801,.T.);
#1553=FACE_BOUND('',#3803,.T.);
#1554=FACE_BOUND('',#3809,.T.);
#1555=FACE_BOUND('',#3815,.T.);
#1556=FACE_BOUND('',#3821,.T.);
#1557=FACE_BOUND('',#3833,.T.);
#1558=FACE_BOUND('',#3834,.T.);
#1559=FACE_BOUND('',#3835,.T.);
#1560=FACE_BOUND('',#3836,.T.);
#1561=FACE_BOUND('',#3837,.T.);
#1562=FACE_BOUND('',#3839,.T.);
#1563=FACE_BOUND('',#3840,.T.);
#1564=FACE_BOUND('',#3841,.T.);
#1565=FACE_BOUND('',#3842,.T.);
#1566=FACE_BOUND('',#3843,.T.);
#1567=FACE_BOUND('',#3845,.T.);
#1568=FACE_BOUND('',#3851,.T.);
#1569=FACE_BOUND('',#3857,.T.);
#1570=FACE_BOUND('',#3863,.T.);
#1571=FACE_BOUND('',#3877,.T.);
#1572=FACE_BOUND('',#3878,.T.);
#1573=FACE_BOUND('',#3879,.T.);
#1574=FACE_BOUND('',#3880,.T.);
#1575=FACE_BOUND('',#3881,.T.);
#1576=FACE_BOUND('',#3882,.T.);
#1577=FACE_BOUND('',#3883,.T.);
#1578=FACE_BOUND('',#3892,.T.);
#1579=FACE_BOUND('',#3893,.T.);
#1580=FACE_BOUND('',#3894,.T.);
#1581=FACE_BOUND('',#3895,.T.);
#1582=FACE_BOUND('',#3896,.T.);
#1583=FACE_BOUND('',#3897,.T.);
#1584=FACE_BOUND('',#3898,.T.);
#1585=FACE_BOUND('',#3902,.T.);
#1586=FACE_BOUND('',#3904,.T.);
#1587=FACE_BOUND('',#3908,.T.);
#1588=FACE_BOUND('',#3910,.T.);
#1589=FACE_BOUND('',#3918,.T.);
#1590=FACE_BOUND('',#3919,.T.);
#1591=FACE_BOUND('',#3920,.T.);
#1592=FACE_BOUND('',#3921,.T.);
#1593=FACE_BOUND('',#3922,.T.);
#1594=FACE_BOUND('',#3924,.T.);
#1595=FACE_BOUND('',#3925,.T.);
#1596=FACE_BOUND('',#3926,.T.);
#1597=FACE_BOUND('',#3927,.T.);
#1598=FACE_BOUND('',#3928,.T.);
#1599=FACE_BOUND('',#3930,.T.);
#1600=FACE_BOUND('',#3936,.T.);
#1601=FACE_BOUND('',#3942,.T.);
#1602=FACE_BOUND('',#3948,.T.);
#1603=FACE_BOUND('',#3960,.T.);
#1604=FACE_BOUND('',#3961,.T.);
#1605=FACE_BOUND('',#3962,.T.);
#1606=FACE_BOUND('',#3963,.T.);
#1607=FACE_BOUND('',#3964,.T.);
#1608=FACE_BOUND('',#3966,.T.);
#1609=FACE_BOUND('',#3967,.T.);
#1610=FACE_BOUND('',#3968,.T.);
#1611=FACE_BOUND('',#3969,.T.);
#1612=FACE_BOUND('',#3970,.T.);
#1613=FACE_BOUND('',#3972,.T.);
#1614=FACE_BOUND('',#3978,.T.);
#1615=FACE_BOUND('',#3984,.T.);
#1616=FACE_BOUND('',#3990,.T.);
#1617=FACE_BOUND('',#4000,.T.);
#1618=FACE_BOUND('',#4003,.T.);
#1619=FACE_BOUND('',#4008,.T.);
#1620=FACE_BOUND('',#4013,.T.);
#1621=FACE_BOUND('',#4065,.T.);
#1622=FACE_BOUND('',#4068,.T.);
#1623=FACE_BOUND('',#4071,.T.);
#1624=FACE_BOUND('',#4074,.T.);
#1625=FACE_BOUND('',#4077,.T.);
#1626=FACE_BOUND('',#4079,.T.);
#1627=FACE_BOUND('',#4083,.T.);
#1628=FACE_BOUND('',#4085,.T.);
#1629=FACE_BOUND('',#4094,.T.);
#1630=FACE_BOUND('',#4096,.T.);
#1631=FACE_BOUND('',#4100,.T.);
#1632=FACE_BOUND('',#4102,.T.);
#1633=FACE_BOUND('',#4106,.T.);
#1634=FACE_BOUND('',#4108,.T.);
#1635=FACE_BOUND('',#4112,.T.);
#1636=FACE_BOUND('',#4114,.T.);
#1637=FACE_BOUND('',#4120,.T.);
#1638=FACE_BOUND('',#4122,.T.);
#1639=FACE_BOUND('',#4123,.T.);
#1640=PLANE('',#14612);
#1641=PLANE('',#14613);
#1642=PLANE('',#14614);
#1643=PLANE('',#14615);
#1644=PLANE('',#14616);
#1645=PLANE('',#14617);
#1646=PLANE('',#14619);
#1647=PLANE('',#14620);
#1648=PLANE('',#14621);
#1649=PLANE('',#14622);
#1650=PLANE('',#14623);
#1651=PLANE('',#14624);
#1652=PLANE('',#14626);
#1653=PLANE('',#14627);
#1654=PLANE('',#14628);
#1655=PLANE('',#14629);
#1656=PLANE('',#14630);
#1657=PLANE('',#14631);
#1658=PLANE('',#14660);
#1659=PLANE('',#14661);
#1660=PLANE('',#14662);
#1661=PLANE('',#14663);
#1662=PLANE('',#14664);
#1663=PLANE('',#14666);
#1664=PLANE('',#14675);
#1665=PLANE('',#14676);
#1666=PLANE('',#14677);
#1667=PLANE('',#14678);
#1668=PLANE('',#14695);
#1669=PLANE('',#14702);
#1670=PLANE('',#14703);
#1671=PLANE('',#14720);
#1672=PLANE('',#14727);
#1673=PLANE('',#14728);
#1674=PLANE('',#14757);
#1675=PLANE('',#14758);
#1676=PLANE('',#14759);
#1677=PLANE('',#14760);
#1678=PLANE('',#14761);
#1679=PLANE('',#14762);
#1680=PLANE('',#14769);
#1681=PLANE('',#14770);
#1682=PLANE('',#14771);
#1683=PLANE('',#14772);
#1684=PLANE('',#14789);
#1685=PLANE('',#14796);
#1686=PLANE('',#14797);
#1687=PLANE('',#14814);
#1688=PLANE('',#14821);
#1689=PLANE('',#14822);
#1690=PLANE('',#14827);
#1691=PLANE('',#14828);
#1692=PLANE('',#14833);
#1693=PLANE('',#14834);
#1694=PLANE('',#14839);
#1695=PLANE('',#14843);
#1696=PLANE('',#14847);
#1697=PLANE('',#14848);
#1698=PLANE('',#14856);
#1699=PLANE('',#14857);
#1700=PLANE('',#14865);
#1701=PLANE('',#14866);
#1702=PLANE('',#14874);
#1703=PLANE('',#14875);
#1704=PLANE('',#14883);
#1705=PLANE('',#14884);
#1706=PLANE('',#14892);
#1707=PLANE('',#14893);
#1708=PLANE('',#14895);
#1709=PLANE('',#14896);
#1710=PLANE('',#14897);
#1711=PLANE('',#14898);
#1712=PLANE('',#14899);
#1713=PLANE('',#14900);
#1714=PLANE('',#14901);
#1715=PLANE('',#14902);
#1716=PLANE('',#14903);
#1717=PLANE('',#14905);
#1718=PLANE('',#14913);
#1719=PLANE('',#14944);
#1720=PLANE('',#14945);
#1721=PLANE('',#14946);
#1722=PLANE('',#14947);
#1723=PLANE('',#14948);
#1724=PLANE('',#14949);
#1725=PLANE('',#14963);
#1726=PLANE('',#14964);
#1727=PLANE('',#14965);
#1728=PLANE('',#14966);
#1729=PLANE('',#14967);
#1730=PLANE('',#14968);
#1731=PLANE('',#14970);
#1732=PLANE('',#14979);
#1733=PLANE('',#14980);
#1734=PLANE('',#14981);
#1735=PLANE('',#14982);
#1736=PLANE('',#14996);
#1737=PLANE('',#14997);
#1738=PLANE('',#14998);
#1739=PLANE('',#14999);
#1740=PLANE('',#15000);
#1741=PLANE('',#15003);
#1742=PLANE('',#15008);
#1743=PLANE('',#15009);
#1744=PLANE('',#15010);
#1745=PLANE('',#15011);
#1746=PLANE('',#15016);
#1747=PLANE('',#15017);
#1748=PLANE('',#15022);
#1749=PLANE('',#15023);
#1750=PLANE('',#15028);
#1751=PLANE('',#15032);
#1752=PLANE('',#15036);
#1753=PLANE('',#15037);
#1754=PLANE('',#15045);
#1755=PLANE('',#15046);
#1756=PLANE('',#15054);
#1757=PLANE('',#15055);
#1758=PLANE('',#15063);
#1759=PLANE('',#15064);
#1760=PLANE('',#15072);
#1761=PLANE('',#15073);
#1762=PLANE('',#15081);
#1763=PLANE('',#15082);
#1764=PLANE('',#15090);
#1765=PLANE('',#15091);
#1766=PLANE('',#15093);
#1767=PLANE('',#15101);
#1768=PLANE('',#15109);
#1769=PLANE('',#15110);
#1770=PLANE('',#15111);
#1771=PLANE('',#15112);
#1772=PLANE('',#15113);
#1773=PLANE('',#15114);
#1774=PLANE('',#15115);
#1775=PLANE('',#15116);
#1776=PLANE('',#15117);
#1777=PLANE('',#15129);
#1778=PLANE('',#15130);
#1779=PLANE('',#15131);
#1780=PLANE('',#15132);
#1781=PLANE('',#15133);
#1782=PLANE('',#15134);
#1783=PLANE('',#15139);
#1784=PLANE('',#15144);
#1785=PLANE('',#15153);
#1786=PLANE('',#15154);
#1787=PLANE('',#15155);
#1788=PLANE('',#15156);
#1789=PLANE('',#15157);
#1790=PLANE('',#15158);
#1791=PLANE('',#15163);
#1792=PLANE('',#15168);
#1793=PLANE('',#15177);
#1794=PLANE('',#15178);
#1795=PLANE('',#15179);
#1796=PLANE('',#15180);
#1797=PLANE('',#15181);
#1798=PLANE('',#15182);
#1799=PLANE('',#15184);
#1800=PLANE('',#15190);
#1801=PLANE('',#15194);
#1802=PLANE('',#15195);
#1803=PLANE('',#15196);
#1804=PLANE('',#15197);
#1805=PLANE('',#15198);
#1806=PLANE('',#15199);
#1807=PLANE('',#15204);
#1808=PLANE('',#15208);
#1809=PLANE('',#15212);
#1810=PLANE('',#15213);
#1811=PLANE('',#15221);
#1812=PLANE('',#15222);
#1813=PLANE('',#15230);
#1814=PLANE('',#15231);
#1815=PLANE('',#15239);
#1816=PLANE('',#15240);
#1817=PLANE('',#15248);
#1818=PLANE('',#15249);
#1819=PLANE('',#15257);
#1820=PLANE('',#15258);
#1821=PLANE('',#15266);
#1822=PLANE('',#15267);
#1823=PLANE('',#15279);
#1824=PLANE('',#15280);
#1825=PLANE('',#15281);
#1826=PLANE('',#15282);
#1827=PLANE('',#15283);
#1828=PLANE('',#15284);
#1829=PLANE('',#15289);
#1830=PLANE('',#15294);
#1831=PLANE('',#15303);
#1832=PLANE('',#15304);
#1833=PLANE('',#15305);
#1834=PLANE('',#15306);
#1835=PLANE('',#15307);
#1836=PLANE('',#15308);
#1837=PLANE('',#15313);
#1838=PLANE('',#15318);
#1839=PLANE('',#15327);
#1840=PLANE('',#15328);
#1841=PLANE('',#15329);
#1842=PLANE('',#15330);
#1843=PLANE('',#15331);
#1844=PLANE('',#15332);
#1845=PLANE('',#15334);
#1846=PLANE('',#15340);
#1847=PLANE('',#15344);
#1848=PLANE('',#15345);
#1849=PLANE('',#15346);
#1850=PLANE('',#15347);
#1851=PLANE('',#15348);
#1852=PLANE('',#15349);
#1853=PLANE('',#15354);
#1854=PLANE('',#15358);
#1855=PLANE('',#15362);
#1856=PLANE('',#15363);
#1857=PLANE('',#15371);
#1858=PLANE('',#15372);
#1859=PLANE('',#15380);
#1860=PLANE('',#15381);
#1861=PLANE('',#15389);
#1862=PLANE('',#15390);
#1863=PLANE('',#15398);
#1864=PLANE('',#15399);
#1865=PLANE('',#15407);
#1866=PLANE('',#15408);
#1867=PLANE('',#15416);
#1868=PLANE('',#15417);
#1869=PLANE('',#15420);
#1870=PLANE('',#15422);
#1871=PLANE('',#15423);
#1872=PLANE('',#15425);
#1873=PLANE('',#15426);
#1874=PLANE('',#15427);
#1875=PLANE('',#15432);
#1876=PLANE('',#15436);
#1877=PLANE('',#15440);
#1878=PLANE('',#15444);
#1879=PLANE('',#15448);
#1880=PLANE('',#15452);
#1881=PLANE('',#15455);
#1882=PLANE('',#15456);
#1883=PLANE('',#15459);
#1884=PLANE('',#15460);
#1885=PLANE('',#15465);
#1886=PLANE('',#15471);
#1887=PLANE('',#15473);
#1888=PLANE('',#15474);
#1889=PLANE('',#15475);
#1890=PLANE('',#15476);
#1891=PLANE('',#15477);
#1892=PLANE('',#15478);
#1893=PLANE('',#15479);
#1894=PLANE('',#15480);
#1895=PLANE('',#15496);
#1896=PLANE('',#15497);
#1897=PLANE('',#15498);
#1898=PLANE('',#15505);
#1899=PLANE('',#15508);
#1900=PLANE('',#15513);
#1901=PLANE('',#15521);
#1902=PLANE('',#15522);
#1903=PLANE('',#15530);
#1904=PLANE('',#15531);
#1905=PLANE('',#15539);
#1906=PLANE('',#15540);
#1907=PLANE('',#15551);
#1908=PLANE('',#15552);
#1909=PLANE('',#15553);
#1910=PLANE('',#15560);
#1911=PLANE('',#15563);
#1912=PLANE('',#15568);
#1913=PLANE('',#15576);
#1914=PLANE('',#15577);
#1915=PLANE('',#15585);
#1916=PLANE('',#15586);
#1917=PLANE('',#15594);
#1918=PLANE('',#15595);
#1919=PLANE('',#15600);
#1920=PLANE('',#15604);
#1921=PLANE('',#15608);
#1922=PLANE('',#15609);
#1923=PLANE('',#15617);
#1924=PLANE('',#15618);
#1925=PLANE('',#15626);
#1926=PLANE('',#15627);
#1927=PLANE('',#15635);
#1928=PLANE('',#15636);
#1929=PLANE('',#15644);
#1930=PLANE('',#15645);
#1931=PLANE('',#15653);
#1932=PLANE('',#15654);
#1933=PLANE('',#15662);
#1934=PLANE('',#15663);
#1935=PLANE('',#15671);
#1936=PLANE('',#15672);
#1937=PLANE('',#15674);
#1938=PLANE('',#15682);
#1939=PLANE('',#15690);
#1940=PLANE('',#15691);
#1941=PLANE('',#15692);
#1942=PLANE('',#15693);
#1943=PLANE('',#15694);
#1944=PLANE('',#15695);
#1945=PLANE('',#15696);
#1946=PLANE('',#15697);
#1947=PLANE('',#15698);
#1948=PLANE('',#15794);
#1949=PLANE('',#15795);
#1950=PLANE('',#15800);
#1951=PLANE('',#15805);
#1952=PLANE('',#15810);
#1953=PLANE('',#15811);
#1954=PLANE('',#15819);
#1955=PLANE('',#15820);
#1956=PLANE('',#15828);
#1957=PLANE('',#15829);
#1958=PLANE('',#15849);
#1959=PLANE('',#15850);
#1960=PLANE('',#15852);
#1961=PLANE('',#15857);
#1962=PLANE('',#15860);
#1963=PLANE('',#15862);
#1964=PLANE('',#15867);
#1965=PLANE('',#15870);
#1966=PLANE('',#15872);
#1967=PLANE('',#15877);
#1968=PLANE('',#15880);
#1969=PLANE('',#15882);
#1970=PLANE('',#15887);
#1971=PLANE('',#15890);
#1972=PLANE('',#15910);
#1973=PLANE('',#15911);
#1974=PLANE('',#15913);
#1975=PLANE('',#15918);
#1976=PLANE('',#15921);
#1977=PLANE('',#15923);
#1978=PLANE('',#15928);
#1979=PLANE('',#15931);
#1980=PLANE('',#15933);
#1981=PLANE('',#15938);
#1982=PLANE('',#15941);
#1983=PLANE('',#15943);
#1984=PLANE('',#15948);
#1985=PLANE('',#15951);
#1986=PLANE('',#15974);
#1987=PLANE('',#15975);
#1988=PLANE('',#15980);
#1989=PLANE('',#15985);
#1990=PLANE('',#15990);
#1991=PLANE('',#15991);
#1992=PLANE('',#15999);
#1993=PLANE('',#16000);
#1994=PLANE('',#16008);
#1995=PLANE('',#16009);
#1996=PLANE('',#16029);
#1997=PLANE('',#16030);
#1998=PLANE('',#16032);
#1999=PLANE('',#16037);
#2000=PLANE('',#16040);
#2001=PLANE('',#16042);
#2002=PLANE('',#16047);
#2003=PLANE('',#16050);
#2004=PLANE('',#16052);
#2005=PLANE('',#16057);
#2006=PLANE('',#16060);
#2007=PLANE('',#16062);
#2008=PLANE('',#16067);
#2009=PLANE('',#16070);
#2010=PLANE('',#16090);
#2011=PLANE('',#16091);
#2012=PLANE('',#16093);
#2013=PLANE('',#16098);
#2014=PLANE('',#16101);
#2015=PLANE('',#16103);
#2016=PLANE('',#16108);
#2017=PLANE('',#16111);
#2018=PLANE('',#16113);
#2019=PLANE('',#16118);
#2020=PLANE('',#16121);
#2021=PLANE('',#16123);
#2022=PLANE('',#16128);
#2023=PLANE('',#16131);
#2024=PLANE('',#16147);
#2025=PLANE('',#16150);
#2026=PLANE('',#16162);
#2027=PLANE('',#16171);
#2028=PLANE('',#16192);
#2029=PLANE('',#16198);
#2030=PLANE('',#16206);
#2031=PLANE('',#16214);
#2032=PLANE('',#16223);
#2033=PLANE('',#16226);
#2034=PLANE('',#16237);
#2035=PLANE('',#16242);
#2036=PLANE('',#16251);
#2037=PLANE('',#16254);
#2038=PLANE('',#16265);
#2039=PLANE('',#16270);
#2040=PLANE('',#16276);
#2041=PLANE('',#16282);
#2042=PLANE('',#16288);
#2043=PLANE('',#16293);
#2044=PLANE('',#16296);
#2045=PLANE('',#16301);
#2046=PLANE('',#16384);
#2047=PLANE('',#16387);
#2048=PLANE('',#16393);
#2049=PLANE('',#16395);
#2050=PLANE('',#16403);
#2051=PLANE('',#16404);
#2052=PLANE('',#16412);
#2053=PLANE('',#16413);
#2054=PLANE('',#16421);
#2055=PLANE('',#16422);
#2056=PLANE('',#16430);
#2057=PLANE('',#16431);
#2058=PLANE('',#16439);
#2059=PLANE('',#16440);
#2060=PLANE('',#16445);
#2061=PLANE('',#16452);
#2062=PLANE('',#16453);
#2063=FACE_OUTER_BOUND('',#2881,.T.);
#2064=FACE_OUTER_BOUND('',#2882,.T.);
#2065=FACE_OUTER_BOUND('',#2883,.T.);
#2066=FACE_OUTER_BOUND('',#2884,.T.);
#2067=FACE_OUTER_BOUND('',#2885,.T.);
#2068=FACE_OUTER_BOUND('',#2886,.T.);
#2069=FACE_OUTER_BOUND('',#2887,.T.);
#2070=FACE_OUTER_BOUND('',#2888,.T.);
#2071=FACE_OUTER_BOUND('',#2889,.T.);
#2072=FACE_OUTER_BOUND('',#2890,.T.);
#2073=FACE_OUTER_BOUND('',#2891,.T.);
#2074=FACE_OUTER_BOUND('',#2892,.T.);
#2075=FACE_OUTER_BOUND('',#2893,.T.);
#2076=FACE_OUTER_BOUND('',#2902,.T.);
#2077=FACE_OUTER_BOUND('',#2911,.T.);
#2078=FACE_OUTER_BOUND('',#2912,.T.);
#2079=FACE_OUTER_BOUND('',#2913,.T.);
#2080=FACE_OUTER_BOUND('',#2914,.T.);
#2081=FACE_OUTER_BOUND('',#2915,.T.);
#2082=FACE_OUTER_BOUND('',#2916,.T.);
#2083=FACE_OUTER_BOUND('',#2917,.T.);
#2084=FACE_OUTER_BOUND('',#2918,.T.);
#2085=FACE_OUTER_BOUND('',#2919,.T.);
#2086=FACE_OUTER_BOUND('',#2920,.T.);
#2087=FACE_OUTER_BOUND('',#2921,.T.);
#2088=FACE_OUTER_BOUND('',#2922,.T.);
#2089=FACE_OUTER_BOUND('',#2923,.T.);
#2090=FACE_OUTER_BOUND('',#2924,.T.);
#2091=FACE_OUTER_BOUND('',#2925,.T.);
#2092=FACE_OUTER_BOUND('',#2926,.T.);
#2093=FACE_OUTER_BOUND('',#2927,.T.);
#2094=FACE_OUTER_BOUND('',#2928,.T.);
#2095=FACE_OUTER_BOUND('',#2929,.T.);
#2096=FACE_OUTER_BOUND('',#2930,.T.);
#2097=FACE_OUTER_BOUND('',#2931,.T.);
#2098=FACE_OUTER_BOUND('',#2932,.T.);
#2099=FACE_OUTER_BOUND('',#2935,.T.);
#2100=FACE_OUTER_BOUND('',#2938,.T.);
#2101=FACE_OUTER_BOUND('',#2939,.T.);
#2102=FACE_OUTER_BOUND('',#2940,.T.);
#2103=FACE_OUTER_BOUND('',#2942,.T.);
#2104=FACE_OUTER_BOUND('',#2950,.T.);
#2105=FACE_OUTER_BOUND('',#2951,.T.);
#2106=FACE_OUTER_BOUND('',#2952,.T.);
#2107=FACE_OUTER_BOUND('',#2953,.T.);
#2108=FACE_OUTER_BOUND('',#2961,.T.);
#2109=FACE_OUTER_BOUND('',#2963,.T.);
#2110=FACE_OUTER_BOUND('',#2964,.T.);
#2111=FACE_OUTER_BOUND('',#2969,.T.);
#2112=FACE_OUTER_BOUND('',#2970,.T.);
#2113=FACE_OUTER_BOUND('',#2971,.T.);
#2114=FACE_OUTER_BOUND('',#2972,.T.);
#2115=FACE_OUTER_BOUND('',#2973,.T.);
#2116=FACE_OUTER_BOUND('',#2974,.T.);
#2117=FACE_OUTER_BOUND('',#2976,.T.);
#2118=FACE_OUTER_BOUND('',#2977,.T.);
#2119=FACE_OUTER_BOUND('',#2978,.T.);
#2120=FACE_OUTER_BOUND('',#2984,.T.);
#2121=FACE_OUTER_BOUND('',#2990,.T.);
#2122=FACE_OUTER_BOUND('',#2991,.T.);
#2123=FACE_OUTER_BOUND('',#2992,.T.);
#2124=FACE_OUTER_BOUND('',#2993,.T.);
#2125=FACE_OUTER_BOUND('',#2994,.T.);
#2126=FACE_OUTER_BOUND('',#2995,.T.);
#2127=FACE_OUTER_BOUND('',#2997,.T.);
#2128=FACE_OUTER_BOUND('',#2998,.T.);
#2129=FACE_OUTER_BOUND('',#2999,.T.);
#2130=FACE_OUTER_BOUND('',#3005,.T.);
#2131=FACE_OUTER_BOUND('',#3011,.T.);
#2132=FACE_OUTER_BOUND('',#3012,.T.);
#2133=FACE_OUTER_BOUND('',#3013,.T.);
#2134=FACE_OUTER_BOUND('',#3014,.T.);
#2135=FACE_OUTER_BOUND('',#3015,.T.);
#2136=FACE_OUTER_BOUND('',#3016,.T.);
#2137=FACE_OUTER_BOUND('',#3017,.T.);
#2138=FACE_OUTER_BOUND('',#3018,.T.);
#2139=FACE_OUTER_BOUND('',#3019,.T.);
#2140=FACE_OUTER_BOUND('',#3020,.T.);
#2141=FACE_OUTER_BOUND('',#3023,.T.);
#2142=FACE_OUTER_BOUND('',#3026,.T.);
#2143=FACE_OUTER_BOUND('',#3027,.T.);
#2144=FACE_OUTER_BOUND('',#3028,.T.);
#2145=FACE_OUTER_BOUND('',#3029,.T.);
#2146=FACE_OUTER_BOUND('',#3037,.T.);
#2147=FACE_OUTER_BOUND('',#3038,.T.);
#2148=FACE_OUTER_BOUND('',#3039,.T.);
#2149=FACE_OUTER_BOUND('',#3047,.T.);
#2150=FACE_OUTER_BOUND('',#3048,.T.);
#2151=FACE_OUTER_BOUND('',#3049,.T.);
#2152=FACE_OUTER_BOUND('',#3054,.T.);
#2153=FACE_OUTER_BOUND('',#3055,.T.);
#2154=FACE_OUTER_BOUND('',#3056,.T.);
#2155=FACE_OUTER_BOUND('',#3057,.T.);
#2156=FACE_OUTER_BOUND('',#3058,.T.);
#2157=FACE_OUTER_BOUND('',#3059,.T.);
#2158=FACE_OUTER_BOUND('',#3061,.T.);
#2159=FACE_OUTER_BOUND('',#3062,.T.);
#2160=FACE_OUTER_BOUND('',#3063,.T.);
#2161=FACE_OUTER_BOUND('',#3069,.T.);
#2162=FACE_OUTER_BOUND('',#3075,.T.);
#2163=FACE_OUTER_BOUND('',#3076,.T.);
#2164=FACE_OUTER_BOUND('',#3077,.T.);
#2165=FACE_OUTER_BOUND('',#3078,.T.);
#2166=FACE_OUTER_BOUND('',#3079,.T.);
#2167=FACE_OUTER_BOUND('',#3080,.T.);
#2168=FACE_OUTER_BOUND('',#3082,.T.);
#2169=FACE_OUTER_BOUND('',#3083,.T.);
#2170=FACE_OUTER_BOUND('',#3084,.T.);
#2171=FACE_OUTER_BOUND('',#3090,.T.);
#2172=FACE_OUTER_BOUND('',#3096,.T.);
#2173=FACE_OUTER_BOUND('',#3097,.T.);
#2174=FACE_OUTER_BOUND('',#3098,.T.);
#2175=FACE_OUTER_BOUND('',#3099,.T.);
#2176=FACE_OUTER_BOUND('',#3100,.T.);
#2177=FACE_OUTER_BOUND('',#3101,.T.);
#2178=FACE_OUTER_BOUND('',#3102,.T.);
#2179=FACE_OUTER_BOUND('',#3103,.T.);
#2180=FACE_OUTER_BOUND('',#3104,.T.);
#2181=FACE_OUTER_BOUND('',#3105,.T.);
#2182=FACE_OUTER_BOUND('',#3106,.T.);
#2183=FACE_OUTER_BOUND('',#3107,.T.);
#2184=FACE_OUTER_BOUND('',#3109,.T.);
#2185=FACE_OUTER_BOUND('',#3111,.T.);
#2186=FACE_OUTER_BOUND('',#3112,.T.);
#2187=FACE_OUTER_BOUND('',#3113,.T.);
#2188=FACE_OUTER_BOUND('',#3115,.T.);
#2189=FACE_OUTER_BOUND('',#3117,.T.);
#2190=FACE_OUTER_BOUND('',#3118,.T.);
#2191=FACE_OUTER_BOUND('',#3119,.T.);
#2192=FACE_OUTER_BOUND('',#3121,.T.);
#2193=FACE_OUTER_BOUND('',#3123,.T.);
#2194=FACE_OUTER_BOUND('',#3124,.T.);
#2195=FACE_OUTER_BOUND('',#3125,.T.);
#2196=FACE_OUTER_BOUND('',#3127,.T.);
#2197=FACE_OUTER_BOUND('',#3129,.T.);
#2198=FACE_OUTER_BOUND('',#3130,.T.);
#2199=FACE_OUTER_BOUND('',#3131,.T.);
#2200=FACE_OUTER_BOUND('',#3133,.T.);
#2201=FACE_OUTER_BOUND('',#3135,.T.);
#2202=FACE_OUTER_BOUND('',#3136,.T.);
#2203=FACE_OUTER_BOUND('',#3137,.T.);
#2204=FACE_OUTER_BOUND('',#3139,.T.);
#2205=FACE_OUTER_BOUND('',#3141,.T.);
#2206=FACE_OUTER_BOUND('',#3142,.T.);
#2207=FACE_OUTER_BOUND('',#3143,.T.);
#2208=FACE_OUTER_BOUND('',#3144,.T.);
#2209=FACE_OUTER_BOUND('',#3145,.T.);
#2210=FACE_OUTER_BOUND('',#3146,.T.);
#2211=FACE_OUTER_BOUND('',#3147,.T.);
#2212=FACE_OUTER_BOUND('',#3148,.T.);
#2213=FACE_OUTER_BOUND('',#3149,.T.);
#2214=FACE_OUTER_BOUND('',#3150,.T.);
#2215=FACE_OUTER_BOUND('',#3151,.T.);
#2216=FACE_OUTER_BOUND('',#3152,.T.);
#2217=FACE_OUTER_BOUND('',#3153,.T.);
#2218=FACE_OUTER_BOUND('',#3154,.T.);
#2219=FACE_OUTER_BOUND('',#3156,.T.);
#2220=FACE_OUTER_BOUND('',#3157,.T.);
#2221=FACE_OUTER_BOUND('',#3158,.T.);
#2222=FACE_OUTER_BOUND('',#3159,.T.);
#2223=FACE_OUTER_BOUND('',#3160,.T.);
#2224=FACE_OUTER_BOUND('',#3161,.T.);
#2225=FACE_OUTER_BOUND('',#3162,.T.);
#2226=FACE_OUTER_BOUND('',#3163,.T.);
#2227=FACE_OUTER_BOUND('',#3164,.T.);
#2228=FACE_OUTER_BOUND('',#3165,.T.);
#2229=FACE_OUTER_BOUND('',#3166,.T.);
#2230=FACE_OUTER_BOUND('',#3167,.T.);
#2231=FACE_OUTER_BOUND('',#3168,.T.);
#2232=FACE_OUTER_BOUND('',#3169,.T.);
#2233=FACE_OUTER_BOUND('',#3170,.T.);
#2234=FACE_OUTER_BOUND('',#3179,.T.);
#2235=FACE_OUTER_BOUND('',#3188,.T.);
#2236=FACE_OUTER_BOUND('',#3189,.T.);
#2237=FACE_OUTER_BOUND('',#3190,.T.);
#2238=FACE_OUTER_BOUND('',#3191,.T.);
#2239=FACE_OUTER_BOUND('',#3192,.T.);
#2240=FACE_OUTER_BOUND('',#3198,.T.);
#2241=FACE_OUTER_BOUND('',#3199,.T.);
#2242=FACE_OUTER_BOUND('',#3200,.T.);
#2243=FACE_OUTER_BOUND('',#3201,.T.);
#2244=FACE_OUTER_BOUND('',#3202,.T.);
#2245=FACE_OUTER_BOUND('',#3204,.T.);
#2246=FACE_OUTER_BOUND('',#3207,.T.);
#2247=FACE_OUTER_BOUND('',#3208,.T.);
#2248=FACE_OUTER_BOUND('',#3209,.T.);
#2249=FACE_OUTER_BOUND('',#3210,.T.);
#2250=FACE_OUTER_BOUND('',#3212,.T.);
#2251=FACE_OUTER_BOUND('',#3215,.T.);
#2252=FACE_OUTER_BOUND('',#3220,.T.);
#2253=FACE_OUTER_BOUND('',#3221,.T.);
#2254=FACE_OUTER_BOUND('',#3222,.T.);
#2255=FACE_OUTER_BOUND('',#3223,.T.);
#2256=FACE_OUTER_BOUND('',#3224,.T.);
#2257=FACE_OUTER_BOUND('',#3225,.T.);
#2258=FACE_OUTER_BOUND('',#3228,.T.);
#2259=FACE_OUTER_BOUND('',#3229,.T.);
#2260=FACE_OUTER_BOUND('',#3230,.T.);
#2261=FACE_OUTER_BOUND('',#3233,.T.);
#2262=FACE_OUTER_BOUND('',#3236,.T.);
#2263=FACE_OUTER_BOUND('',#3237,.T.);
#2264=FACE_OUTER_BOUND('',#3238,.T.);
#2265=FACE_OUTER_BOUND('',#3239,.T.);
#2266=FACE_OUTER_BOUND('',#3240,.T.);
#2267=FACE_OUTER_BOUND('',#3243,.T.);
#2268=FACE_OUTER_BOUND('',#3248,.T.);
#2269=FACE_OUTER_BOUND('',#3249,.T.);
#2270=FACE_OUTER_BOUND('',#3250,.T.);
#2271=FACE_OUTER_BOUND('',#3251,.T.);
#2272=FACE_OUTER_BOUND('',#3252,.T.);
#2273=FACE_OUTER_BOUND('',#3253,.T.);
#2274=FACE_OUTER_BOUND('',#3254,.T.);
#2275=FACE_OUTER_BOUND('',#3255,.T.);
#2276=FACE_OUTER_BOUND('',#3256,.T.);
#2277=FACE_OUTER_BOUND('',#3257,.T.);
#2278=FACE_OUTER_BOUND('',#3258,.T.);
#2279=FACE_OUTER_BOUND('',#3259,.T.);
#2280=FACE_OUTER_BOUND('',#3260,.T.);
#2281=FACE_OUTER_BOUND('',#3262,.T.);
#2282=FACE_OUTER_BOUND('',#3264,.T.);
#2283=FACE_OUTER_BOUND('',#3265,.T.);
#2284=FACE_OUTER_BOUND('',#3266,.T.);
#2285=FACE_OUTER_BOUND('',#3268,.T.);
#2286=FACE_OUTER_BOUND('',#3270,.T.);
#2287=FACE_OUTER_BOUND('',#3271,.T.);
#2288=FACE_OUTER_BOUND('',#3272,.T.);
#2289=FACE_OUTER_BOUND('',#3274,.T.);
#2290=FACE_OUTER_BOUND('',#3276,.T.);
#2291=FACE_OUTER_BOUND('',#3277,.T.);
#2292=FACE_OUTER_BOUND('',#3278,.T.);
#2293=FACE_OUTER_BOUND('',#3280,.T.);
#2294=FACE_OUTER_BOUND('',#3282,.T.);
#2295=FACE_OUTER_BOUND('',#3283,.T.);
#2296=FACE_OUTER_BOUND('',#3284,.T.);
#2297=FACE_OUTER_BOUND('',#3286,.T.);
#2298=FACE_OUTER_BOUND('',#3288,.T.);
#2299=FACE_OUTER_BOUND('',#3289,.T.);
#2300=FACE_OUTER_BOUND('',#3290,.T.);
#2301=FACE_OUTER_BOUND('',#3292,.T.);
#2302=FACE_OUTER_BOUND('',#3294,.T.);
#2303=FACE_OUTER_BOUND('',#3295,.T.);
#2304=FACE_OUTER_BOUND('',#3296,.T.);
#2305=FACE_OUTER_BOUND('',#3298,.T.);
#2306=FACE_OUTER_BOUND('',#3300,.T.);
#2307=FACE_OUTER_BOUND('',#3301,.T.);
#2308=FACE_OUTER_BOUND('',#3302,.T.);
#2309=FACE_OUTER_BOUND('',#3303,.T.);
#2310=FACE_OUTER_BOUND('',#3304,.T.);
#2311=FACE_OUTER_BOUND('',#3306,.T.);
#2312=FACE_OUTER_BOUND('',#3307,.T.);
#2313=FACE_OUTER_BOUND('',#3308,.T.);
#2314=FACE_OUTER_BOUND('',#3309,.T.);
#2315=FACE_OUTER_BOUND('',#3310,.T.);
#2316=FACE_OUTER_BOUND('',#3311,.T.);
#2317=FACE_OUTER_BOUND('',#3312,.T.);
#2318=FACE_OUTER_BOUND('',#3313,.T.);
#2319=FACE_OUTER_BOUND('',#3314,.T.);
#2320=FACE_OUTER_BOUND('',#3315,.T.);
#2321=FACE_OUTER_BOUND('',#3316,.T.);
#2322=FACE_OUTER_BOUND('',#3317,.T.);
#2323=FACE_OUTER_BOUND('',#3318,.T.);
#2324=FACE_OUTER_BOUND('',#3319,.T.);
#2325=FACE_OUTER_BOUND('',#3320,.T.);
#2326=FACE_OUTER_BOUND('',#3321,.T.);
#2327=FACE_OUTER_BOUND('',#3322,.T.);
#2328=FACE_OUTER_BOUND('',#3326,.T.);
#2329=FACE_OUTER_BOUND('',#3327,.T.);
#2330=FACE_OUTER_BOUND('',#3331,.T.);
#2331=FACE_OUTER_BOUND('',#3332,.T.);
#2332=FACE_OUTER_BOUND('',#3333,.T.);
#2333=FACE_OUTER_BOUND('',#3334,.T.);
#2334=FACE_OUTER_BOUND('',#3336,.T.);
#2335=FACE_OUTER_BOUND('',#3337,.T.);
#2336=FACE_OUTER_BOUND('',#3339,.T.);
#2337=FACE_OUTER_BOUND('',#3340,.T.);
#2338=FACE_OUTER_BOUND('',#3341,.T.);
#2339=FACE_OUTER_BOUND('',#3342,.T.);
#2340=FACE_OUTER_BOUND('',#3343,.T.);
#2341=FACE_OUTER_BOUND('',#3344,.T.);
#2342=FACE_OUTER_BOUND('',#3345,.T.);
#2343=FACE_OUTER_BOUND('',#3346,.T.);
#2344=FACE_OUTER_BOUND('',#3350,.T.);
#2345=FACE_OUTER_BOUND('',#3354,.T.);
#2346=FACE_OUTER_BOUND('',#3355,.T.);
#2347=FACE_OUTER_BOUND('',#3357,.T.);
#2348=FACE_OUTER_BOUND('',#3358,.T.);
#2349=FACE_OUTER_BOUND('',#3360,.T.);
#2350=FACE_OUTER_BOUND('',#3361,.T.);
#2351=FACE_OUTER_BOUND('',#3362,.T.);
#2352=FACE_OUTER_BOUND('',#3363,.T.);
#2353=FACE_OUTER_BOUND('',#3364,.T.);
#2354=FACE_OUTER_BOUND('',#3365,.T.);
#2355=FACE_OUTER_BOUND('',#3366,.T.);
#2356=FACE_OUTER_BOUND('',#3367,.T.);
#2357=FACE_OUTER_BOUND('',#3371,.T.);
#2358=FACE_OUTER_BOUND('',#3375,.T.);
#2359=FACE_OUTER_BOUND('',#3376,.T.);
#2360=FACE_OUTER_BOUND('',#3377,.T.);
#2361=FACE_OUTER_BOUND('',#3378,.T.);
#2362=FACE_OUTER_BOUND('',#3380,.T.);
#2363=FACE_OUTER_BOUND('',#3382,.T.);
#2364=FACE_OUTER_BOUND('',#3384,.T.);
#2365=FACE_OUTER_BOUND('',#3386,.T.);
#2366=FACE_OUTER_BOUND('',#3387,.T.);
#2367=FACE_OUTER_BOUND('',#3388,.T.);
#2368=FACE_OUTER_BOUND('',#3389,.T.);
#2369=FACE_OUTER_BOUND('',#3390,.T.);
#2370=FACE_OUTER_BOUND('',#3391,.T.);
#2371=FACE_OUTER_BOUND('',#3392,.T.);
#2372=FACE_OUTER_BOUND('',#3393,.T.);
#2373=FACE_OUTER_BOUND('',#3394,.T.);
#2374=FACE_OUTER_BOUND('',#3396,.T.);
#2375=FACE_OUTER_BOUND('',#3398,.T.);
#2376=FACE_OUTER_BOUND('',#3399,.T.);
#2377=FACE_OUTER_BOUND('',#3400,.T.);
#2378=FACE_OUTER_BOUND('',#3402,.T.);
#2379=FACE_OUTER_BOUND('',#3404,.T.);
#2380=FACE_OUTER_BOUND('',#3405,.T.);
#2381=FACE_OUTER_BOUND('',#3406,.T.);
#2382=FACE_OUTER_BOUND('',#3408,.T.);
#2383=FACE_OUTER_BOUND('',#3410,.T.);
#2384=FACE_OUTER_BOUND('',#3411,.T.);
#2385=FACE_OUTER_BOUND('',#3412,.T.);
#2386=FACE_OUTER_BOUND('',#3414,.T.);
#2387=FACE_OUTER_BOUND('',#3416,.T.);
#2388=FACE_OUTER_BOUND('',#3417,.T.);
#2389=FACE_OUTER_BOUND('',#3418,.T.);
#2390=FACE_OUTER_BOUND('',#3420,.T.);
#2391=FACE_OUTER_BOUND('',#3422,.T.);
#2392=FACE_OUTER_BOUND('',#3423,.T.);
#2393=FACE_OUTER_BOUND('',#3424,.T.);
#2394=FACE_OUTER_BOUND('',#3426,.T.);
#2395=FACE_OUTER_BOUND('',#3428,.T.);
#2396=FACE_OUTER_BOUND('',#3429,.T.);
#2397=FACE_OUTER_BOUND('',#3430,.T.);
#2398=FACE_OUTER_BOUND('',#3432,.T.);
#2399=FACE_OUTER_BOUND('',#3434,.T.);
#2400=FACE_OUTER_BOUND('',#3435,.T.);
#2401=FACE_OUTER_BOUND('',#3436,.T.);
#2402=FACE_OUTER_BOUND('',#3437,.T.);
#2403=FACE_OUTER_BOUND('',#3438,.T.);
#2404=FACE_OUTER_BOUND('',#3442,.T.);
#2405=FACE_OUTER_BOUND('',#3443,.T.);
#2406=FACE_OUTER_BOUND('',#3447,.T.);
#2407=FACE_OUTER_BOUND('',#3448,.T.);
#2408=FACE_OUTER_BOUND('',#3449,.T.);
#2409=FACE_OUTER_BOUND('',#3450,.T.);
#2410=FACE_OUTER_BOUND('',#3452,.T.);
#2411=FACE_OUTER_BOUND('',#3453,.T.);
#2412=FACE_OUTER_BOUND('',#3455,.T.);
#2413=FACE_OUTER_BOUND('',#3456,.T.);
#2414=FACE_OUTER_BOUND('',#3457,.T.);
#2415=FACE_OUTER_BOUND('',#3458,.T.);
#2416=FACE_OUTER_BOUND('',#3459,.T.);
#2417=FACE_OUTER_BOUND('',#3460,.T.);
#2418=FACE_OUTER_BOUND('',#3461,.T.);
#2419=FACE_OUTER_BOUND('',#3462,.T.);
#2420=FACE_OUTER_BOUND('',#3466,.T.);
#2421=FACE_OUTER_BOUND('',#3470,.T.);
#2422=FACE_OUTER_BOUND('',#3471,.T.);
#2423=FACE_OUTER_BOUND('',#3473,.T.);
#2424=FACE_OUTER_BOUND('',#3474,.T.);
#2425=FACE_OUTER_BOUND('',#3476,.T.);
#2426=FACE_OUTER_BOUND('',#3477,.T.);
#2427=FACE_OUTER_BOUND('',#3478,.T.);
#2428=FACE_OUTER_BOUND('',#3479,.T.);
#2429=FACE_OUTER_BOUND('',#3480,.T.);
#2430=FACE_OUTER_BOUND('',#3481,.T.);
#2431=FACE_OUTER_BOUND('',#3482,.T.);
#2432=FACE_OUTER_BOUND('',#3483,.T.);
#2433=FACE_OUTER_BOUND('',#3487,.T.);
#2434=FACE_OUTER_BOUND('',#3491,.T.);
#2435=FACE_OUTER_BOUND('',#3492,.T.);
#2436=FACE_OUTER_BOUND('',#3493,.T.);
#2437=FACE_OUTER_BOUND('',#3494,.T.);
#2438=FACE_OUTER_BOUND('',#3496,.T.);
#2439=FACE_OUTER_BOUND('',#3498,.T.);
#2440=FACE_OUTER_BOUND('',#3500,.T.);
#2441=FACE_OUTER_BOUND('',#3502,.T.);
#2442=FACE_OUTER_BOUND('',#3503,.T.);
#2443=FACE_OUTER_BOUND('',#3504,.T.);
#2444=FACE_OUTER_BOUND('',#3505,.T.);
#2445=FACE_OUTER_BOUND('',#3506,.T.);
#2446=FACE_OUTER_BOUND('',#3507,.T.);
#2447=FACE_OUTER_BOUND('',#3508,.T.);
#2448=FACE_OUTER_BOUND('',#3509,.T.);
#2449=FACE_OUTER_BOUND('',#3510,.T.);
#2450=FACE_OUTER_BOUND('',#3512,.T.);
#2451=FACE_OUTER_BOUND('',#3514,.T.);
#2452=FACE_OUTER_BOUND('',#3515,.T.);
#2453=FACE_OUTER_BOUND('',#3516,.T.);
#2454=FACE_OUTER_BOUND('',#3518,.T.);
#2455=FACE_OUTER_BOUND('',#3520,.T.);
#2456=FACE_OUTER_BOUND('',#3521,.T.);
#2457=FACE_OUTER_BOUND('',#3522,.T.);
#2458=FACE_OUTER_BOUND('',#3524,.T.);
#2459=FACE_OUTER_BOUND('',#3526,.T.);
#2460=FACE_OUTER_BOUND('',#3527,.T.);
#2461=FACE_OUTER_BOUND('',#3528,.T.);
#2462=FACE_OUTER_BOUND('',#3530,.T.);
#2463=FACE_OUTER_BOUND('',#3532,.T.);
#2464=FACE_OUTER_BOUND('',#3533,.T.);
#2465=FACE_OUTER_BOUND('',#3534,.T.);
#2466=FACE_OUTER_BOUND('',#3536,.T.);
#2467=FACE_OUTER_BOUND('',#3538,.T.);
#2468=FACE_OUTER_BOUND('',#3539,.T.);
#2469=FACE_OUTER_BOUND('',#3540,.T.);
#2470=FACE_OUTER_BOUND('',#3542,.T.);
#2471=FACE_OUTER_BOUND('',#3544,.T.);
#2472=FACE_OUTER_BOUND('',#3545,.T.);
#2473=FACE_OUTER_BOUND('',#3546,.T.);
#2474=FACE_OUTER_BOUND('',#3548,.T.);
#2475=FACE_OUTER_BOUND('',#3550,.T.);
#2476=FACE_OUTER_BOUND('',#3551,.T.);
#2477=FACE_OUTER_BOUND('',#3552,.T.);
#2478=FACE_OUTER_BOUND('',#3553,.T.);
#2479=FACE_OUTER_BOUND('',#3554,.T.);
#2480=FACE_OUTER_BOUND('',#3555,.T.);
#2481=FACE_OUTER_BOUND('',#3557,.T.);
#2482=FACE_OUTER_BOUND('',#3558,.T.);
#2483=FACE_OUTER_BOUND('',#3560,.T.);
#2484=FACE_OUTER_BOUND('',#3561,.T.);
#2485=FACE_OUTER_BOUND('',#3563,.T.);
#2486=FACE_OUTER_BOUND('',#3564,.T.);
#2487=FACE_OUTER_BOUND('',#3566,.T.);
#2488=FACE_OUTER_BOUND('',#3567,.T.);
#2489=FACE_OUTER_BOUND('',#3569,.T.);
#2490=FACE_OUTER_BOUND('',#3570,.T.);
#2491=FACE_OUTER_BOUND('',#3572,.T.);
#2492=FACE_OUTER_BOUND('',#3574,.T.);
#2493=FACE_OUTER_BOUND('',#3575,.T.);
#2494=FACE_OUTER_BOUND('',#3576,.T.);
#2495=FACE_OUTER_BOUND('',#3577,.T.);
#2496=FACE_OUTER_BOUND('',#3578,.T.);
#2497=FACE_OUTER_BOUND('',#3580,.T.);
#2498=FACE_OUTER_BOUND('',#3582,.T.);
#2499=FACE_OUTER_BOUND('',#3584,.T.);
#2500=FACE_OUTER_BOUND('',#3586,.T.);
#2501=FACE_OUTER_BOUND('',#3587,.T.);
#2502=FACE_OUTER_BOUND('',#3588,.T.);
#2503=FACE_OUTER_BOUND('',#3589,.T.);
#2504=FACE_OUTER_BOUND('',#3590,.T.);
#2505=FACE_OUTER_BOUND('',#3591,.T.);
#2506=FACE_OUTER_BOUND('',#3592,.T.);
#2507=FACE_OUTER_BOUND('',#3593,.T.);
#2508=FACE_OUTER_BOUND('',#3594,.T.);
#2509=FACE_OUTER_BOUND('',#3596,.T.);
#2510=FACE_OUTER_BOUND('',#3597,.T.);
#2511=FACE_OUTER_BOUND('',#3598,.T.);
#2512=FACE_OUTER_BOUND('',#3599,.T.);
#2513=FACE_OUTER_BOUND('',#3600,.T.);
#2514=FACE_OUTER_BOUND('',#3601,.T.);
#2515=FACE_OUTER_BOUND('',#3602,.T.);
#2516=FACE_OUTER_BOUND('',#3603,.T.);
#2517=FACE_OUTER_BOUND('',#3604,.T.);
#2518=FACE_OUTER_BOUND('',#3605,.T.);
#2519=FACE_OUTER_BOUND('',#3606,.T.);
#2520=FACE_OUTER_BOUND('',#3610,.T.);
#2521=FACE_OUTER_BOUND('',#3611,.T.);
#2522=FACE_OUTER_BOUND('',#3612,.T.);
#2523=FACE_OUTER_BOUND('',#3613,.T.);
#2524=FACE_OUTER_BOUND('',#3617,.T.);
#2525=FACE_OUTER_BOUND('',#3618,.T.);
#2526=FACE_OUTER_BOUND('',#3619,.T.);
#2527=FACE_OUTER_BOUND('',#3621,.T.);
#2528=FACE_OUTER_BOUND('',#3623,.T.);
#2529=FACE_OUTER_BOUND('',#3624,.T.);
#2530=FACE_OUTER_BOUND('',#3625,.T.);
#2531=FACE_OUTER_BOUND('',#3627,.T.);
#2532=FACE_OUTER_BOUND('',#3629,.T.);
#2533=FACE_OUTER_BOUND('',#3630,.T.);
#2534=FACE_OUTER_BOUND('',#3631,.T.);
#2535=FACE_OUTER_BOUND('',#3633,.T.);
#2536=FACE_OUTER_BOUND('',#3635,.T.);
#2537=FACE_OUTER_BOUND('',#3636,.T.);
#2538=FACE_OUTER_BOUND('',#3637,.T.);
#2539=FACE_OUTER_BOUND('',#3638,.T.);
#2540=FACE_OUTER_BOUND('',#3639,.T.);
#2541=FACE_OUTER_BOUND('',#3640,.T.);
#2542=FACE_OUTER_BOUND('',#3641,.T.);
#2543=FACE_OUTER_BOUND('',#3642,.T.);
#2544=FACE_OUTER_BOUND('',#3643,.T.);
#2545=FACE_OUTER_BOUND('',#3647,.T.);
#2546=FACE_OUTER_BOUND('',#3648,.T.);
#2547=FACE_OUTER_BOUND('',#3649,.T.);
#2548=FACE_OUTER_BOUND('',#3650,.T.);
#2549=FACE_OUTER_BOUND('',#3654,.T.);
#2550=FACE_OUTER_BOUND('',#3655,.T.);
#2551=FACE_OUTER_BOUND('',#3656,.T.);
#2552=FACE_OUTER_BOUND('',#3658,.T.);
#2553=FACE_OUTER_BOUND('',#3660,.T.);
#2554=FACE_OUTER_BOUND('',#3661,.T.);
#2555=FACE_OUTER_BOUND('',#3662,.T.);
#2556=FACE_OUTER_BOUND('',#3664,.T.);
#2557=FACE_OUTER_BOUND('',#3666,.T.);
#2558=FACE_OUTER_BOUND('',#3667,.T.);
#2559=FACE_OUTER_BOUND('',#3668,.T.);
#2560=FACE_OUTER_BOUND('',#3670,.T.);
#2561=FACE_OUTER_BOUND('',#3672,.T.);
#2562=FACE_OUTER_BOUND('',#3673,.T.);
#2563=FACE_OUTER_BOUND('',#3674,.T.);
#2564=FACE_OUTER_BOUND('',#3675,.T.);
#2565=FACE_OUTER_BOUND('',#3676,.T.);
#2566=FACE_OUTER_BOUND('',#3677,.T.);
#2567=FACE_OUTER_BOUND('',#3679,.T.);
#2568=FACE_OUTER_BOUND('',#3681,.T.);
#2569=FACE_OUTER_BOUND('',#3682,.T.);
#2570=FACE_OUTER_BOUND('',#3683,.T.);
#2571=FACE_OUTER_BOUND('',#3685,.T.);
#2572=FACE_OUTER_BOUND('',#3687,.T.);
#2573=FACE_OUTER_BOUND('',#3688,.T.);
#2574=FACE_OUTER_BOUND('',#3689,.T.);
#2575=FACE_OUTER_BOUND('',#3691,.T.);
#2576=FACE_OUTER_BOUND('',#3693,.T.);
#2577=FACE_OUTER_BOUND('',#3694,.T.);
#2578=FACE_OUTER_BOUND('',#3695,.T.);
#2579=FACE_OUTER_BOUND('',#3697,.T.);
#2580=FACE_OUTER_BOUND('',#3699,.T.);
#2581=FACE_OUTER_BOUND('',#3700,.T.);
#2582=FACE_OUTER_BOUND('',#3701,.T.);
#2583=FACE_OUTER_BOUND('',#3703,.T.);
#2584=FACE_OUTER_BOUND('',#3705,.T.);
#2585=FACE_OUTER_BOUND('',#3706,.T.);
#2586=FACE_OUTER_BOUND('',#3707,.T.);
#2587=FACE_OUTER_BOUND('',#3709,.T.);
#2588=FACE_OUTER_BOUND('',#3711,.T.);
#2589=FACE_OUTER_BOUND('',#3712,.T.);
#2590=FACE_OUTER_BOUND('',#3713,.T.);
#2591=FACE_OUTER_BOUND('',#3715,.T.);
#2592=FACE_OUTER_BOUND('',#3717,.T.);
#2593=FACE_OUTER_BOUND('',#3718,.T.);
#2594=FACE_OUTER_BOUND('',#3719,.T.);
#2595=FACE_OUTER_BOUND('',#3721,.T.);
#2596=FACE_OUTER_BOUND('',#3723,.T.);
#2597=FACE_OUTER_BOUND('',#3724,.T.);
#2598=FACE_OUTER_BOUND('',#3725,.T.);
#2599=FACE_OUTER_BOUND('',#3726,.T.);
#2600=FACE_OUTER_BOUND('',#3727,.T.);
#2601=FACE_OUTER_BOUND('',#3729,.T.);
#2602=FACE_OUTER_BOUND('',#3730,.T.);
#2603=FACE_OUTER_BOUND('',#3731,.T.);
#2604=FACE_OUTER_BOUND('',#3732,.T.);
#2605=FACE_OUTER_BOUND('',#3733,.T.);
#2606=FACE_OUTER_BOUND('',#3734,.T.);
#2607=FACE_OUTER_BOUND('',#3735,.T.);
#2608=FACE_OUTER_BOUND('',#3736,.T.);
#2609=FACE_OUTER_BOUND('',#3737,.T.);
#2610=FACE_OUTER_BOUND('',#3738,.T.);
#2611=FACE_OUTER_BOUND('',#3739,.T.);
#2612=FACE_OUTER_BOUND('',#3740,.T.);
#2613=FACE_OUTER_BOUND('',#3741,.T.);
#2614=FACE_OUTER_BOUND('',#3742,.T.);
#2615=FACE_OUTER_BOUND('',#3743,.T.);
#2616=FACE_OUTER_BOUND('',#3744,.T.);
#2617=FACE_OUTER_BOUND('',#3745,.T.);
#2618=FACE_OUTER_BOUND('',#3746,.T.);
#2619=FACE_OUTER_BOUND('',#3747,.T.);
#2620=FACE_OUTER_BOUND('',#3748,.T.);
#2621=FACE_OUTER_BOUND('',#3749,.T.);
#2622=FACE_OUTER_BOUND('',#3757,.T.);
#2623=FACE_OUTER_BOUND('',#3758,.T.);
#2624=FACE_OUTER_BOUND('',#3759,.T.);
#2625=FACE_OUTER_BOUND('',#3760,.T.);
#2626=FACE_OUTER_BOUND('',#3761,.T.);
#2627=FACE_OUTER_BOUND('',#3762,.T.);
#2628=FACE_OUTER_BOUND('',#3763,.T.);
#2629=FACE_OUTER_BOUND('',#3764,.T.);
#2630=FACE_OUTER_BOUND('',#3772,.T.);
#2631=FACE_OUTER_BOUND('',#3773,.T.);
#2632=FACE_OUTER_BOUND('',#3774,.T.);
#2633=FACE_OUTER_BOUND('',#3776,.T.);
#2634=FACE_OUTER_BOUND('',#3778,.T.);
#2635=FACE_OUTER_BOUND('',#3779,.T.);
#2636=FACE_OUTER_BOUND('',#3780,.T.);
#2637=FACE_OUTER_BOUND('',#3782,.T.);
#2638=FACE_OUTER_BOUND('',#3784,.T.);
#2639=FACE_OUTER_BOUND('',#3785,.T.);
#2640=FACE_OUTER_BOUND('',#3786,.T.);
#2641=FACE_OUTER_BOUND('',#3787,.T.);
#2642=FACE_OUTER_BOUND('',#3788,.T.);
#2643=FACE_OUTER_BOUND('',#3789,.T.);
#2644=FACE_OUTER_BOUND('',#3790,.T.);
#2645=FACE_OUTER_BOUND('',#3796,.T.);
#2646=FACE_OUTER_BOUND('',#3802,.T.);
#2647=FACE_OUTER_BOUND('',#3804,.T.);
#2648=FACE_OUTER_BOUND('',#3805,.T.);
#2649=FACE_OUTER_BOUND('',#3806,.T.);
#2650=FACE_OUTER_BOUND('',#3807,.T.);
#2651=FACE_OUTER_BOUND('',#3808,.T.);
#2652=FACE_OUTER_BOUND('',#3810,.T.);
#2653=FACE_OUTER_BOUND('',#3811,.T.);
#2654=FACE_OUTER_BOUND('',#3812,.T.);
#2655=FACE_OUTER_BOUND('',#3813,.T.);
#2656=FACE_OUTER_BOUND('',#3814,.T.);
#2657=FACE_OUTER_BOUND('',#3816,.T.);
#2658=FACE_OUTER_BOUND('',#3817,.T.);
#2659=FACE_OUTER_BOUND('',#3818,.T.);
#2660=FACE_OUTER_BOUND('',#3819,.T.);
#2661=FACE_OUTER_BOUND('',#3820,.T.);
#2662=FACE_OUTER_BOUND('',#3822,.T.);
#2663=FACE_OUTER_BOUND('',#3823,.T.);
#2664=FACE_OUTER_BOUND('',#3824,.T.);
#2665=FACE_OUTER_BOUND('',#3825,.T.);
#2666=FACE_OUTER_BOUND('',#3826,.T.);
#2667=FACE_OUTER_BOUND('',#3827,.T.);
#2668=FACE_OUTER_BOUND('',#3828,.T.);
#2669=FACE_OUTER_BOUND('',#3829,.T.);
#2670=FACE_OUTER_BOUND('',#3830,.T.);
#2671=FACE_OUTER_BOUND('',#3831,.T.);
#2672=FACE_OUTER_BOUND('',#3832,.T.);
#2673=FACE_OUTER_BOUND('',#3838,.T.);
#2674=FACE_OUTER_BOUND('',#3844,.T.);
#2675=FACE_OUTER_BOUND('',#3846,.T.);
#2676=FACE_OUTER_BOUND('',#3847,.T.);
#2677=FACE_OUTER_BOUND('',#3848,.T.);
#2678=FACE_OUTER_BOUND('',#3849,.T.);
#2679=FACE_OUTER_BOUND('',#3850,.T.);
#2680=FACE_OUTER_BOUND('',#3852,.T.);
#2681=FACE_OUTER_BOUND('',#3853,.T.);
#2682=FACE_OUTER_BOUND('',#3854,.T.);
#2683=FACE_OUTER_BOUND('',#3855,.T.);
#2684=FACE_OUTER_BOUND('',#3856,.T.);
#2685=FACE_OUTER_BOUND('',#3858,.T.);
#2686=FACE_OUTER_BOUND('',#3859,.T.);
#2687=FACE_OUTER_BOUND('',#3860,.T.);
#2688=FACE_OUTER_BOUND('',#3861,.T.);
#2689=FACE_OUTER_BOUND('',#3862,.T.);
#2690=FACE_OUTER_BOUND('',#3864,.T.);
#2691=FACE_OUTER_BOUND('',#3865,.T.);
#2692=FACE_OUTER_BOUND('',#3866,.T.);
#2693=FACE_OUTER_BOUND('',#3867,.T.);
#2694=FACE_OUTER_BOUND('',#3868,.T.);
#2695=FACE_OUTER_BOUND('',#3869,.T.);
#2696=FACE_OUTER_BOUND('',#3870,.T.);
#2697=FACE_OUTER_BOUND('',#3871,.T.);
#2698=FACE_OUTER_BOUND('',#3872,.T.);
#2699=FACE_OUTER_BOUND('',#3873,.T.);
#2700=FACE_OUTER_BOUND('',#3874,.T.);
#2701=FACE_OUTER_BOUND('',#3875,.T.);
#2702=FACE_OUTER_BOUND('',#3876,.T.);
#2703=FACE_OUTER_BOUND('',#3884,.T.);
#2704=FACE_OUTER_BOUND('',#3885,.T.);
#2705=FACE_OUTER_BOUND('',#3886,.T.);
#2706=FACE_OUTER_BOUND('',#3887,.T.);
#2707=FACE_OUTER_BOUND('',#3888,.T.);
#2708=FACE_OUTER_BOUND('',#3889,.T.);
#2709=FACE_OUTER_BOUND('',#3890,.T.);
#2710=FACE_OUTER_BOUND('',#3891,.T.);
#2711=FACE_OUTER_BOUND('',#3899,.T.);
#2712=FACE_OUTER_BOUND('',#3900,.T.);
#2713=FACE_OUTER_BOUND('',#3901,.T.);
#2714=FACE_OUTER_BOUND('',#3903,.T.);
#2715=FACE_OUTER_BOUND('',#3905,.T.);
#2716=FACE_OUTER_BOUND('',#3906,.T.);
#2717=FACE_OUTER_BOUND('',#3907,.T.);
#2718=FACE_OUTER_BOUND('',#3909,.T.);
#2719=FACE_OUTER_BOUND('',#3911,.T.);
#2720=FACE_OUTER_BOUND('',#3912,.T.);
#2721=FACE_OUTER_BOUND('',#3913,.T.);
#2722=FACE_OUTER_BOUND('',#3914,.T.);
#2723=FACE_OUTER_BOUND('',#3915,.T.);
#2724=FACE_OUTER_BOUND('',#3916,.T.);
#2725=FACE_OUTER_BOUND('',#3917,.T.);
#2726=FACE_OUTER_BOUND('',#3923,.T.);
#2727=FACE_OUTER_BOUND('',#3929,.T.);
#2728=FACE_OUTER_BOUND('',#3931,.T.);
#2729=FACE_OUTER_BOUND('',#3932,.T.);
#2730=FACE_OUTER_BOUND('',#3933,.T.);
#2731=FACE_OUTER_BOUND('',#3934,.T.);
#2732=FACE_OUTER_BOUND('',#3935,.T.);
#2733=FACE_OUTER_BOUND('',#3937,.T.);
#2734=FACE_OUTER_BOUND('',#3938,.T.);
#2735=FACE_OUTER_BOUND('',#3939,.T.);
#2736=FACE_OUTER_BOUND('',#3940,.T.);
#2737=FACE_OUTER_BOUND('',#3941,.T.);
#2738=FACE_OUTER_BOUND('',#3943,.T.);
#2739=FACE_OUTER_BOUND('',#3944,.T.);
#2740=FACE_OUTER_BOUND('',#3945,.T.);
#2741=FACE_OUTER_BOUND('',#3946,.T.);
#2742=FACE_OUTER_BOUND('',#3947,.T.);
#2743=FACE_OUTER_BOUND('',#3949,.T.);
#2744=FACE_OUTER_BOUND('',#3950,.T.);
#2745=FACE_OUTER_BOUND('',#3951,.T.);
#2746=FACE_OUTER_BOUND('',#3952,.T.);
#2747=FACE_OUTER_BOUND('',#3953,.T.);
#2748=FACE_OUTER_BOUND('',#3954,.T.);
#2749=FACE_OUTER_BOUND('',#3955,.T.);
#2750=FACE_OUTER_BOUND('',#3956,.T.);
#2751=FACE_OUTER_BOUND('',#3957,.T.);
#2752=FACE_OUTER_BOUND('',#3958,.T.);
#2753=FACE_OUTER_BOUND('',#3959,.T.);
#2754=FACE_OUTER_BOUND('',#3965,.T.);
#2755=FACE_OUTER_BOUND('',#3971,.T.);
#2756=FACE_OUTER_BOUND('',#3973,.T.);
#2757=FACE_OUTER_BOUND('',#3974,.T.);
#2758=FACE_OUTER_BOUND('',#3975,.T.);
#2759=FACE_OUTER_BOUND('',#3976,.T.);
#2760=FACE_OUTER_BOUND('',#3977,.T.);
#2761=FACE_OUTER_BOUND('',#3979,.T.);
#2762=FACE_OUTER_BOUND('',#3980,.T.);
#2763=FACE_OUTER_BOUND('',#3981,.T.);
#2764=FACE_OUTER_BOUND('',#3982,.T.);
#2765=FACE_OUTER_BOUND('',#3983,.T.);
#2766=FACE_OUTER_BOUND('',#3985,.T.);
#2767=FACE_OUTER_BOUND('',#3986,.T.);
#2768=FACE_OUTER_BOUND('',#3987,.T.);
#2769=FACE_OUTER_BOUND('',#3988,.T.);
#2770=FACE_OUTER_BOUND('',#3989,.T.);
#2771=FACE_OUTER_BOUND('',#3991,.T.);
#2772=FACE_OUTER_BOUND('',#3992,.T.);
#2773=FACE_OUTER_BOUND('',#3993,.T.);
#2774=FACE_OUTER_BOUND('',#3994,.T.);
#2775=FACE_OUTER_BOUND('',#3995,.T.);
#2776=FACE_OUTER_BOUND('',#3996,.T.);
#2777=FACE_OUTER_BOUND('',#3997,.T.);
#2778=FACE_OUTER_BOUND('',#3998,.T.);
#2779=FACE_OUTER_BOUND('',#3999,.T.);
#2780=FACE_OUTER_BOUND('',#4001,.T.);
#2781=FACE_OUTER_BOUND('',#4002,.T.);
#2782=FACE_OUTER_BOUND('',#4004,.T.);
#2783=FACE_OUTER_BOUND('',#4005,.T.);
#2784=FACE_OUTER_BOUND('',#4006,.T.);
#2785=FACE_OUTER_BOUND('',#4007,.T.);
#2786=FACE_OUTER_BOUND('',#4009,.T.);
#2787=FACE_OUTER_BOUND('',#4010,.T.);
#2788=FACE_OUTER_BOUND('',#4011,.T.);
#2789=FACE_OUTER_BOUND('',#4012,.T.);
#2790=FACE_OUTER_BOUND('',#4014,.T.);
#2791=FACE_OUTER_BOUND('',#4015,.T.);
#2792=FACE_OUTER_BOUND('',#4016,.T.);
#2793=FACE_OUTER_BOUND('',#4017,.T.);
#2794=FACE_OUTER_BOUND('',#4018,.T.);
#2795=FACE_OUTER_BOUND('',#4019,.T.);
#2796=FACE_OUTER_BOUND('',#4020,.T.);
#2797=FACE_OUTER_BOUND('',#4021,.T.);
#2798=FACE_OUTER_BOUND('',#4022,.T.);
#2799=FACE_OUTER_BOUND('',#4023,.T.);
#2800=FACE_OUTER_BOUND('',#4024,.T.);
#2801=FACE_OUTER_BOUND('',#4025,.T.);
#2802=FACE_OUTER_BOUND('',#4026,.T.);
#2803=FACE_OUTER_BOUND('',#4027,.T.);
#2804=FACE_OUTER_BOUND('',#4028,.T.);
#2805=FACE_OUTER_BOUND('',#4029,.T.);
#2806=FACE_OUTER_BOUND('',#4030,.T.);
#2807=FACE_OUTER_BOUND('',#4031,.T.);
#2808=FACE_OUTER_BOUND('',#4032,.T.);
#2809=FACE_OUTER_BOUND('',#4033,.T.);
#2810=FACE_OUTER_BOUND('',#4034,.T.);
#2811=FACE_OUTER_BOUND('',#4035,.T.);
#2812=FACE_OUTER_BOUND('',#4036,.T.);
#2813=FACE_OUTER_BOUND('',#4037,.T.);
#2814=FACE_OUTER_BOUND('',#4038,.T.);
#2815=FACE_OUTER_BOUND('',#4039,.T.);
#2816=FACE_OUTER_BOUND('',#4040,.T.);
#2817=FACE_OUTER_BOUND('',#4041,.T.);
#2818=FACE_OUTER_BOUND('',#4042,.T.);
#2819=FACE_OUTER_BOUND('',#4043,.T.);
#2820=FACE_OUTER_BOUND('',#4044,.T.);
#2821=FACE_OUTER_BOUND('',#4045,.T.);
#2822=FACE_OUTER_BOUND('',#4046,.T.);
#2823=FACE_OUTER_BOUND('',#4047,.T.);
#2824=FACE_OUTER_BOUND('',#4048,.T.);
#2825=FACE_OUTER_BOUND('',#4049,.T.);
#2826=FACE_OUTER_BOUND('',#4050,.T.);
#2827=FACE_OUTER_BOUND('',#4051,.T.);
#2828=FACE_OUTER_BOUND('',#4052,.T.);
#2829=FACE_OUTER_BOUND('',#4053,.T.);
#2830=FACE_OUTER_BOUND('',#4054,.T.);
#2831=FACE_OUTER_BOUND('',#4055,.T.);
#2832=FACE_OUTER_BOUND('',#4056,.T.);
#2833=FACE_OUTER_BOUND('',#4057,.T.);
#2834=FACE_OUTER_BOUND('',#4058,.T.);
#2835=FACE_OUTER_BOUND('',#4059,.T.);
#2836=FACE_OUTER_BOUND('',#4060,.T.);
#2837=FACE_OUTER_BOUND('',#4061,.T.);
#2838=FACE_OUTER_BOUND('',#4062,.T.);
#2839=FACE_OUTER_BOUND('',#4063,.T.);
#2840=FACE_OUTER_BOUND('',#4064,.T.);
#2841=FACE_OUTER_BOUND('',#4066,.T.);
#2842=FACE_OUTER_BOUND('',#4067,.T.);
#2843=FACE_OUTER_BOUND('',#4069,.T.);
#2844=FACE_OUTER_BOUND('',#4070,.T.);
#2845=FACE_OUTER_BOUND('',#4072,.T.);
#2846=FACE_OUTER_BOUND('',#4073,.T.);
#2847=FACE_OUTER_BOUND('',#4075,.T.);
#2848=FACE_OUTER_BOUND('',#4076,.T.);
#2849=FACE_OUTER_BOUND('',#4078,.T.);
#2850=FACE_OUTER_BOUND('',#4080,.T.);
#2851=FACE_OUTER_BOUND('',#4081,.T.);
#2852=FACE_OUTER_BOUND('',#4082,.T.);
#2853=FACE_OUTER_BOUND('',#4084,.T.);
#2854=FACE_OUTER_BOUND('',#4086,.T.);
#2855=FACE_OUTER_BOUND('',#4087,.T.);
#2856=FACE_OUTER_BOUND('',#4088,.T.);
#2857=FACE_OUTER_BOUND('',#4089,.T.);
#2858=FACE_OUTER_BOUND('',#4090,.T.);
#2859=FACE_OUTER_BOUND('',#4091,.T.);
#2860=FACE_OUTER_BOUND('',#4092,.T.);
#2861=FACE_OUTER_BOUND('',#4093,.T.);
#2862=FACE_OUTER_BOUND('',#4095,.T.);
#2863=FACE_OUTER_BOUND('',#4097,.T.);
#2864=FACE_OUTER_BOUND('',#4098,.T.);
#2865=FACE_OUTER_BOUND('',#4099,.T.);
#2866=FACE_OUTER_BOUND('',#4101,.T.);
#2867=FACE_OUTER_BOUND('',#4103,.T.);
#2868=FACE_OUTER_BOUND('',#4104,.T.);
#2869=FACE_OUTER_BOUND('',#4105,.T.);
#2870=FACE_OUTER_BOUND('',#4107,.T.);
#2871=FACE_OUTER_BOUND('',#4109,.T.);
#2872=FACE_OUTER_BOUND('',#4110,.T.);
#2873=FACE_OUTER_BOUND('',#4111,.T.);
#2874=FACE_OUTER_BOUND('',#4113,.T.);
#2875=FACE_OUTER_BOUND('',#4115,.T.);
#2876=FACE_OUTER_BOUND('',#4116,.T.);
#2877=FACE_OUTER_BOUND('',#4117,.T.);
#2878=FACE_OUTER_BOUND('',#4118,.T.);
#2879=FACE_OUTER_BOUND('',#4119,.T.);
#2880=FACE_OUTER_BOUND('',#4121,.T.);
#2881=EDGE_LOOP('',(#8972,#8973,#8974,#8975));
#2882=EDGE_LOOP('',(#8976,#8977,#8978,#8979));
#2883=EDGE_LOOP('',(#8980,#8981,#8982,#8983));
#2884=EDGE_LOOP('',(#8984,#8985,#8986,#8987));
#2885=EDGE_LOOP('',(#8988,#8989,#8990,#8991));
#2886=EDGE_LOOP('',(#8992,#8993,#8994,#8995));
#2887=EDGE_LOOP('',(#8996,#8997,#8998,#8999));
#2888=EDGE_LOOP('',(#9000,#9001,#9002,#9003));
#2889=EDGE_LOOP('',(#9004,#9005,#9006,#9007));
#2890=EDGE_LOOP('',(#9008,#9009,#9010,#9011));
#2891=EDGE_LOOP('',(#9012,#9013,#9014,#9015));
#2892=EDGE_LOOP('',(#9016,#9017,#9018,#9019));
#2893=EDGE_LOOP('',(#9020,#9021,#9022,#9023));
#2894=EDGE_LOOP('',(#9024));
#2895=EDGE_LOOP('',(#9025));
#2896=EDGE_LOOP('',(#9026));
#2897=EDGE_LOOP('',(#9027));
#2898=EDGE_LOOP('',(#9028));
#2899=EDGE_LOOP('',(#9029));
#2900=EDGE_LOOP('',(#9030));
#2901=EDGE_LOOP('',(#9031));
#2902=EDGE_LOOP('',(#9032,#9033,#9034,#9035));
#2903=EDGE_LOOP('',(#9036));
#2904=EDGE_LOOP('',(#9037));
#2905=EDGE_LOOP('',(#9038));
#2906=EDGE_LOOP('',(#9039));
#2907=EDGE_LOOP('',(#9040));
#2908=EDGE_LOOP('',(#9041));
#2909=EDGE_LOOP('',(#9042));
#2910=EDGE_LOOP('',(#9043));
#2911=EDGE_LOOP('',(#9044,#9045,#9046,#9047));
#2912=EDGE_LOOP('',(#9048,#9049,#9050,#9051));
#2913=EDGE_LOOP('',(#9052,#9053,#9054,#9055));
#2914=EDGE_LOOP('',(#9056,#9057,#9058,#9059));
#2915=EDGE_LOOP('',(#9060,#9061,#9062,#9063));
#2916=EDGE_LOOP('',(#9064,#9065,#9066,#9067));
#2917=EDGE_LOOP('',(#9068,#9069,#9070,#9071));
#2918=EDGE_LOOP('',(#9072,#9073,#9074,#9075));
#2919=EDGE_LOOP('',(#9076,#9077,#9078,#9079));
#2920=EDGE_LOOP('',(#9080,#9081,#9082,#9083));
#2921=EDGE_LOOP('',(#9084,#9085,#9086,#9087));
#2922=EDGE_LOOP('',(#9088,#9089,#9090,#9091));
#2923=EDGE_LOOP('',(#9092,#9093,#9094,#9095));
#2924=EDGE_LOOP('',(#9096,#9097,#9098,#9099));
#2925=EDGE_LOOP('',(#9100,#9101,#9102,#9103));
#2926=EDGE_LOOP('',(#9104,#9105,#9106,#9107));
#2927=EDGE_LOOP('',(#9108,#9109,#9110,#9111));
#2928=EDGE_LOOP('',(#9112,#9113,#9114,#9115));
#2929=EDGE_LOOP('',(#9116,#9117,#9118,#9119));
#2930=EDGE_LOOP('',(#9120,#9121,#9122,#9123));
#2931=EDGE_LOOP('',(#9124,#9125,#9126,#9127));
#2932=EDGE_LOOP('',(#9128,#9129,#9130,#9131));
#2933=EDGE_LOOP('',(#9132));
#2934=EDGE_LOOP('',(#9133));
#2935=EDGE_LOOP('',(#9134,#9135,#9136,#9137));
#2936=EDGE_LOOP('',(#9138));
#2937=EDGE_LOOP('',(#9139));
#2938=EDGE_LOOP('',(#9140,#9141,#9142,#9143));
#2939=EDGE_LOOP('',(#9144,#9145,#9146,#9147));
#2940=EDGE_LOOP('',(#9148,#9149,#9150,#9151,#9152,#9153,#9154,#9155));
#2941=EDGE_LOOP('',(#9156));
#2942=EDGE_LOOP('',(#9157,#9158,#9159,#9160));
#2943=EDGE_LOOP('',(#9161));
#2944=EDGE_LOOP('',(#9162));
#2945=EDGE_LOOP('',(#9163));
#2946=EDGE_LOOP('',(#9164));
#2947=EDGE_LOOP('',(#9165));
#2948=EDGE_LOOP('',(#9166));
#2949=EDGE_LOOP('',(#9167));
#2950=EDGE_LOOP('',(#9168,#9169,#9170,#9171));
#2951=EDGE_LOOP('',(#9172,#9173,#9174,#9175));
#2952=EDGE_LOOP('',(#9176,#9177,#9178,#9179));
#2953=EDGE_LOOP('',(#9180,#9181,#9182,#9183));
#2954=EDGE_LOOP('',(#9184));
#2955=EDGE_LOOP('',(#9185));
#2956=EDGE_LOOP('',(#9186));
#2957=EDGE_LOOP('',(#9187));
#2958=EDGE_LOOP('',(#9188));
#2959=EDGE_LOOP('',(#9189));
#2960=EDGE_LOOP('',(#9190));
#2961=EDGE_LOOP('',(#9191,#9192,#9193,#9194,#9195,#9196,#9197,#9198));
#2962=EDGE_LOOP('',(#9199));
#2963=EDGE_LOOP('',(#9200,#9201,#9202,#9203));
#2964=EDGE_LOOP('',(#9204,#9205,#9206,#9207));
#2965=EDGE_LOOP('',(#9208));
#2966=EDGE_LOOP('',(#9209));
#2967=EDGE_LOOP('',(#9210));
#2968=EDGE_LOOP('',(#9211));
#2969=EDGE_LOOP('',(#9212,#9213,#9214,#9215));
#2970=EDGE_LOOP('',(#9216,#9217,#9218,#9219));
#2971=EDGE_LOOP('',(#9220,#9221,#9222,#9223));
#2972=EDGE_LOOP('',(#9224,#9225,#9226,#9227));
#2973=EDGE_LOOP('',(#9228,#9229,#9230,#9231));
#2974=EDGE_LOOP('',(#9232));
#2975=EDGE_LOOP('',(#9233));
#2976=EDGE_LOOP('',(#9234,#9235,#9236,#9237));
#2977=EDGE_LOOP('',(#9238,#9239,#9240,#9241));
#2978=EDGE_LOOP('',(#9242));
#2979=EDGE_LOOP('',(#9243));
#2980=EDGE_LOOP('',(#9244));
#2981=EDGE_LOOP('',(#9245));
#2982=EDGE_LOOP('',(#9246));
#2983=EDGE_LOOP('',(#9247));
#2984=EDGE_LOOP('',(#9248));
#2985=EDGE_LOOP('',(#9249));
#2986=EDGE_LOOP('',(#9250));
#2987=EDGE_LOOP('',(#9251));
#2988=EDGE_LOOP('',(#9252));
#2989=EDGE_LOOP('',(#9253));
#2990=EDGE_LOOP('',(#9254,#9255,#9256,#9257));
#2991=EDGE_LOOP('',(#9258,#9259,#9260,#9261));
#2992=EDGE_LOOP('',(#9262,#9263,#9264,#9265));
#2993=EDGE_LOOP('',(#9266,#9267,#9268,#9269));
#2994=EDGE_LOOP('',(#9270,#9271,#9272,#9273));
#2995=EDGE_LOOP('',(#9274));
#2996=EDGE_LOOP('',(#9275));
#2997=EDGE_LOOP('',(#9276,#9277,#9278,#9279));
#2998=EDGE_LOOP('',(#9280,#9281,#9282,#9283));
#2999=EDGE_LOOP('',(#9284));
#3000=EDGE_LOOP('',(#9285));
#3001=EDGE_LOOP('',(#9286));
#3002=EDGE_LOOP('',(#9287));
#3003=EDGE_LOOP('',(#9288));
#3004=EDGE_LOOP('',(#9289));
#3005=EDGE_LOOP('',(#9290));
#3006=EDGE_LOOP('',(#9291));
#3007=EDGE_LOOP('',(#9292));
#3008=EDGE_LOOP('',(#9293));
#3009=EDGE_LOOP('',(#9294));
#3010=EDGE_LOOP('',(#9295));
#3011=EDGE_LOOP('',(#9296,#9297,#9298,#9299));
#3012=EDGE_LOOP('',(#9300,#9301,#9302,#9303));
#3013=EDGE_LOOP('',(#9304,#9305,#9306,#9307));
#3014=EDGE_LOOP('',(#9308,#9309,#9310,#9311));
#3015=EDGE_LOOP('',(#9312,#9313,#9314,#9315));
#3016=EDGE_LOOP('',(#9316,#9317,#9318,#9319));
#3017=EDGE_LOOP('',(#9320,#9321,#9322,#9323));
#3018=EDGE_LOOP('',(#9324,#9325,#9326,#9327));
#3019=EDGE_LOOP('',(#9328,#9329,#9330,#9331));
#3020=EDGE_LOOP('',(#9332,#9333,#9334,#9335));
#3021=EDGE_LOOP('',(#9336));
#3022=EDGE_LOOP('',(#9337));
#3023=EDGE_LOOP('',(#9338,#9339,#9340,#9341));
#3024=EDGE_LOOP('',(#9342));
#3025=EDGE_LOOP('',(#9343));
#3026=EDGE_LOOP('',(#9344,#9345,#9346,#9347));
#3027=EDGE_LOOP('',(#9348,#9349,#9350,#9351));
#3028=EDGE_LOOP('',(#9352,#9353,#9354,#9355,#9356,#9357,#9358,#9359));
#3029=EDGE_LOOP('',(#9360,#9361,#9362,#9363));
#3030=EDGE_LOOP('',(#9364));
#3031=EDGE_LOOP('',(#9365));
#3032=EDGE_LOOP('',(#9366));
#3033=EDGE_LOOP('',(#9367));
#3034=EDGE_LOOP('',(#9368));
#3035=EDGE_LOOP('',(#9369));
#3036=EDGE_LOOP('',(#9370));
#3037=EDGE_LOOP('',(#9371,#9372,#9373,#9374));
#3038=EDGE_LOOP('',(#9375,#9376,#9377,#9378));
#3039=EDGE_LOOP('',(#9379,#9380,#9381,#9382));
#3040=EDGE_LOOP('',(#9383));
#3041=EDGE_LOOP('',(#9384));
#3042=EDGE_LOOP('',(#9385));
#3043=EDGE_LOOP('',(#9386));
#3044=EDGE_LOOP('',(#9387));
#3045=EDGE_LOOP('',(#9388));
#3046=EDGE_LOOP('',(#9389));
#3047=EDGE_LOOP('',(#9390,#9391,#9392,#9393,#9394,#9395,#9396,#9397));
#3048=EDGE_LOOP('',(#9398,#9399,#9400,#9401));
#3049=EDGE_LOOP('',(#9402,#9403,#9404,#9405));
#3050=EDGE_LOOP('',(#9406));
#3051=EDGE_LOOP('',(#9407));
#3052=EDGE_LOOP('',(#9408));
#3053=EDGE_LOOP('',(#9409));
#3054=EDGE_LOOP('',(#9410,#9411,#9412,#9413));
#3055=EDGE_LOOP('',(#9414,#9415,#9416,#9417));
#3056=EDGE_LOOP('',(#9418,#9419,#9420,#9421));
#3057=EDGE_LOOP('',(#9422,#9423,#9424,#9425));
#3058=EDGE_LOOP('',(#9426,#9427,#9428,#9429));
#3059=EDGE_LOOP('',(#9430));
#3060=EDGE_LOOP('',(#9431));
#3061=EDGE_LOOP('',(#9432,#9433,#9434,#9435));
#3062=EDGE_LOOP('',(#9436,#9437,#9438,#9439));
#3063=EDGE_LOOP('',(#9440));
#3064=EDGE_LOOP('',(#9441));
#3065=EDGE_LOOP('',(#9442));
#3066=EDGE_LOOP('',(#9443));
#3067=EDGE_LOOP('',(#9444));
#3068=EDGE_LOOP('',(#9445));
#3069=EDGE_LOOP('',(#9446));
#3070=EDGE_LOOP('',(#9447));
#3071=EDGE_LOOP('',(#9448));
#3072=EDGE_LOOP('',(#9449));
#3073=EDGE_LOOP('',(#9450));
#3074=EDGE_LOOP('',(#9451));
#3075=EDGE_LOOP('',(#9452,#9453,#9454,#9455));
#3076=EDGE_LOOP('',(#9456,#9457,#9458,#9459));
#3077=EDGE_LOOP('',(#9460,#9461,#9462,#9463));
#3078=EDGE_LOOP('',(#9464,#9465,#9466,#9467));
#3079=EDGE_LOOP('',(#9468,#9469,#9470,#9471));
#3080=EDGE_LOOP('',(#9472));
#3081=EDGE_LOOP('',(#9473));
#3082=EDGE_LOOP('',(#9474,#9475,#9476,#9477));
#3083=EDGE_LOOP('',(#9478,#9479,#9480,#9481));
#3084=EDGE_LOOP('',(#9482));
#3085=EDGE_LOOP('',(#9483));
#3086=EDGE_LOOP('',(#9484));
#3087=EDGE_LOOP('',(#9485));
#3088=EDGE_LOOP('',(#9486));
#3089=EDGE_LOOP('',(#9487));
#3090=EDGE_LOOP('',(#9488));
#3091=EDGE_LOOP('',(#9489));
#3092=EDGE_LOOP('',(#9490));
#3093=EDGE_LOOP('',(#9491));
#3094=EDGE_LOOP('',(#9492));
#3095=EDGE_LOOP('',(#9493));
#3096=EDGE_LOOP('',(#9494,#9495,#9496,#9497));
#3097=EDGE_LOOP('',(#9498));
#3098=EDGE_LOOP('',(#9499));
#3099=EDGE_LOOP('',(#9500,#9501,#9502,#9503));
#3100=EDGE_LOOP('',(#9504));
#3101=EDGE_LOOP('',(#9505));
#3102=EDGE_LOOP('',(#9506,#9507,#9508,#9509));
#3103=EDGE_LOOP('',(#9510));
#3104=EDGE_LOOP('',(#9511,#9512,#9513,#9514));
#3105=EDGE_LOOP('',(#9515));
#3106=EDGE_LOOP('',(#9516,#9517,#9518,#9519));
#3107=EDGE_LOOP('',(#9520));
#3108=EDGE_LOOP('',(#9521));
#3109=EDGE_LOOP('',(#9522));
#3110=EDGE_LOOP('',(#9523));
#3111=EDGE_LOOP('',(#9524,#9525,#9526,#9527));
#3112=EDGE_LOOP('',(#9528,#9529,#9530,#9531));
#3113=EDGE_LOOP('',(#9532));
#3114=EDGE_LOOP('',(#9533));
#3115=EDGE_LOOP('',(#9534));
#3116=EDGE_LOOP('',(#9535));
#3117=EDGE_LOOP('',(#9536,#9537,#9538,#9539));
#3118=EDGE_LOOP('',(#9540,#9541,#9542,#9543));
#3119=EDGE_LOOP('',(#9544));
#3120=EDGE_LOOP('',(#9545));
#3121=EDGE_LOOP('',(#9546));
#3122=EDGE_LOOP('',(#9547));
#3123=EDGE_LOOP('',(#9548,#9549,#9550,#9551));
#3124=EDGE_LOOP('',(#9552,#9553,#9554,#9555));
#3125=EDGE_LOOP('',(#9556));
#3126=EDGE_LOOP('',(#9557));
#3127=EDGE_LOOP('',(#9558));
#3128=EDGE_LOOP('',(#9559));
#3129=EDGE_LOOP('',(#9560,#9561,#9562,#9563));
#3130=EDGE_LOOP('',(#9564,#9565,#9566,#9567));
#3131=EDGE_LOOP('',(#9568));
#3132=EDGE_LOOP('',(#9569));
#3133=EDGE_LOOP('',(#9570));
#3134=EDGE_LOOP('',(#9571));
#3135=EDGE_LOOP('',(#9572,#9573,#9574,#9575));
#3136=EDGE_LOOP('',(#9576,#9577,#9578,#9579));
#3137=EDGE_LOOP('',(#9580));
#3138=EDGE_LOOP('',(#9581));
#3139=EDGE_LOOP('',(#9582));
#3140=EDGE_LOOP('',(#9583));
#3141=EDGE_LOOP('',(#9584,#9585,#9586,#9587));
#3142=EDGE_LOOP('',(#9588,#9589,#9590,#9591));
#3143=EDGE_LOOP('',(#9592,#9593,#9594,#9595));
#3144=EDGE_LOOP('',(#9596,#9597,#9598,#9599));
#3145=EDGE_LOOP('',(#9600,#9601,#9602,#9603));
#3146=EDGE_LOOP('',(#9604,#9605,#9606,#9607));
#3147=EDGE_LOOP('',(#9608,#9609,#9610,#9611,#9612,#9613));
#3148=EDGE_LOOP('',(#9614,#9615,#9616,#9617,#9618,#9619));
#3149=EDGE_LOOP('',(#9620));
#3150=EDGE_LOOP('',(#9621));
#3151=EDGE_LOOP('',(#9622,#9623,#9624,#9625));
#3152=EDGE_LOOP('',(#9626,#9627,#9628,#9629));
#3153=EDGE_LOOP('',(#9630,#9631,#9632,#9633));
#3154=EDGE_LOOP('',(#9634));
#3155=EDGE_LOOP('',(#9635));
#3156=EDGE_LOOP('',(#9636,#9637,#9638,#9639));
#3157=EDGE_LOOP('',(#9640,#9641,#9642,#9643));
#3158=EDGE_LOOP('',(#9644,#9645,#9646,#9647));
#3159=EDGE_LOOP('',(#9648,#9649,#9650,#9651));
#3160=EDGE_LOOP('',(#9652,#9653,#9654,#9655));
#3161=EDGE_LOOP('',(#9656,#9657,#9658,#9659));
#3162=EDGE_LOOP('',(#9660,#9661,#9662,#9663));
#3163=EDGE_LOOP('',(#9664,#9665,#9666,#9667));
#3164=EDGE_LOOP('',(#9668,#9669,#9670,#9671));
#3165=EDGE_LOOP('',(#9672,#9673,#9674,#9675));
#3166=EDGE_LOOP('',(#9676,#9677,#9678,#9679));
#3167=EDGE_LOOP('',(#9680,#9681,#9682,#9683));
#3168=EDGE_LOOP('',(#9684,#9685,#9686,#9687));
#3169=EDGE_LOOP('',(#9688,#9689,#9690,#9691));
#3170=EDGE_LOOP('',(#9692,#9693,#9694,#9695));
#3171=EDGE_LOOP('',(#9696));
#3172=EDGE_LOOP('',(#9697));
#3173=EDGE_LOOP('',(#9698));
#3174=EDGE_LOOP('',(#9699));
#3175=EDGE_LOOP('',(#9700));
#3176=EDGE_LOOP('',(#9701));
#3177=EDGE_LOOP('',(#9702));
#3178=EDGE_LOOP('',(#9703));
#3179=EDGE_LOOP('',(#9704,#9705,#9706,#9707));
#3180=EDGE_LOOP('',(#9708));
#3181=EDGE_LOOP('',(#9709));
#3182=EDGE_LOOP('',(#9710));
#3183=EDGE_LOOP('',(#9711));
#3184=EDGE_LOOP('',(#9712));
#3185=EDGE_LOOP('',(#9713));
#3186=EDGE_LOOP('',(#9714));
#3187=EDGE_LOOP('',(#9715));
#3188=EDGE_LOOP('',(#9716,#9717,#9718,#9719));
#3189=EDGE_LOOP('',(#9720,#9721,#9722,#9723));
#3190=EDGE_LOOP('',(#9724,#9725,#9726,#9727));
#3191=EDGE_LOOP('',(#9728,#9729,#9730,#9731));
#3192=EDGE_LOOP('',(#9732,#9733,#9734,#9735));
#3193=EDGE_LOOP('',(#9736,#9737,#9738,#9739));
#3194=EDGE_LOOP('',(#9740));
#3195=EDGE_LOOP('',(#9741));
#3196=EDGE_LOOP('',(#9742));
#3197=EDGE_LOOP('',(#9743));
#3198=EDGE_LOOP('',(#9744,#9745,#9746,#9747));
#3199=EDGE_LOOP('',(#9748,#9749,#9750,#9751));
#3200=EDGE_LOOP('',(#9752,#9753,#9754,#9755));
#3201=EDGE_LOOP('',(#9756,#9757,#9758,#9759));
#3202=EDGE_LOOP('',(#9760,#9761,#9762,#9763));
#3203=EDGE_LOOP('',(#9764));
#3204=EDGE_LOOP('',(#9765,#9766,#9767,#9768));
#3205=EDGE_LOOP('',(#9769));
#3206=EDGE_LOOP('',(#9770));
#3207=EDGE_LOOP('',(#9771,#9772,#9773,#9774));
#3208=EDGE_LOOP('',(#9775,#9776,#9777,#9778));
#3209=EDGE_LOOP('',(#9779,#9780,#9781,#9782));
#3210=EDGE_LOOP('',(#9783,#9784,#9785,#9786));
#3211=EDGE_LOOP('',(#9787));
#3212=EDGE_LOOP('',(#9788,#9789,#9790,#9791));
#3213=EDGE_LOOP('',(#9792));
#3214=EDGE_LOOP('',(#9793));
#3215=EDGE_LOOP('',(#9794,#9795,#9796,#9797));
#3216=EDGE_LOOP('',(#9798));
#3217=EDGE_LOOP('',(#9799));
#3218=EDGE_LOOP('',(#9800));
#3219=EDGE_LOOP('',(#9801));
#3220=EDGE_LOOP('',(#9802,#9803,#9804,#9805));
#3221=EDGE_LOOP('',(#9806,#9807,#9808,#9809));
#3222=EDGE_LOOP('',(#9810,#9811,#9812,#9813));
#3223=EDGE_LOOP('',(#9814,#9815,#9816,#9817));
#3224=EDGE_LOOP('',(#9818,#9819,#9820,#9821));
#3225=EDGE_LOOP('',(#9822,#9823,#9824,#9825));
#3226=EDGE_LOOP('',(#9826));
#3227=EDGE_LOOP('',(#9827));
#3228=EDGE_LOOP('',(#9828,#9829,#9830,#9831));
#3229=EDGE_LOOP('',(#9832,#9833,#9834,#9835));
#3230=EDGE_LOOP('',(#9836,#9837,#9838,#9839));
#3231=EDGE_LOOP('',(#9840));
#3232=EDGE_LOOP('',(#9841));
#3233=EDGE_LOOP('',(#9842,#9843,#9844,#9845));
#3234=EDGE_LOOP('',(#9846));
#3235=EDGE_LOOP('',(#9847));
#3236=EDGE_LOOP('',(#9848,#9849,#9850,#9851,#9852,#9853,#9854,#9855));
#3237=EDGE_LOOP('',(#9856,#9857,#9858,#9859));
#3238=EDGE_LOOP('',(#9860,#9861,#9862,#9863));
#3239=EDGE_LOOP('',(#9864,#9865,#9866,#9867,#9868,#9869,#9870,#9871));
#3240=EDGE_LOOP('',(#9872,#9873,#9874,#9875));
#3241=EDGE_LOOP('',(#9876));
#3242=EDGE_LOOP('',(#9877));
#3243=EDGE_LOOP('',(#9878,#9879,#9880,#9881));
#3244=EDGE_LOOP('',(#9882));
#3245=EDGE_LOOP('',(#9883));
#3246=EDGE_LOOP('',(#9884));
#3247=EDGE_LOOP('',(#9885));
#3248=EDGE_LOOP('',(#9886,#9887,#9888,#9889));
#3249=EDGE_LOOP('',(#9890,#9891,#9892,#9893));
#3250=EDGE_LOOP('',(#9894));
#3251=EDGE_LOOP('',(#9895));
#3252=EDGE_LOOP('',(#9896,#9897,#9898,#9899));
#3253=EDGE_LOOP('',(#9900));
#3254=EDGE_LOOP('',(#9901));
#3255=EDGE_LOOP('',(#9902,#9903,#9904,#9905));
#3256=EDGE_LOOP('',(#9906));
#3257=EDGE_LOOP('',(#9907,#9908,#9909,#9910));
#3258=EDGE_LOOP('',(#9911));
#3259=EDGE_LOOP('',(#9912,#9913,#9914,#9915));
#3260=EDGE_LOOP('',(#9916));
#3261=EDGE_LOOP('',(#9917));
#3262=EDGE_LOOP('',(#9918));
#3263=EDGE_LOOP('',(#9919));
#3264=EDGE_LOOP('',(#9920,#9921,#9922,#9923));
#3265=EDGE_LOOP('',(#9924,#9925,#9926,#9927));
#3266=EDGE_LOOP('',(#9928));
#3267=EDGE_LOOP('',(#9929));
#3268=EDGE_LOOP('',(#9930));
#3269=EDGE_LOOP('',(#9931));
#3270=EDGE_LOOP('',(#9932,#9933,#9934,#9935));
#3271=EDGE_LOOP('',(#9936,#9937,#9938,#9939));
#3272=EDGE_LOOP('',(#9940));
#3273=EDGE_LOOP('',(#9941));
#3274=EDGE_LOOP('',(#9942));
#3275=EDGE_LOOP('',(#9943));
#3276=EDGE_LOOP('',(#9944,#9945,#9946,#9947));
#3277=EDGE_LOOP('',(#9948,#9949,#9950,#9951));
#3278=EDGE_LOOP('',(#9952));
#3279=EDGE_LOOP('',(#9953));
#3280=EDGE_LOOP('',(#9954));
#3281=EDGE_LOOP('',(#9955));
#3282=EDGE_LOOP('',(#9956,#9957,#9958,#9959));
#3283=EDGE_LOOP('',(#9960,#9961,#9962,#9963));
#3284=EDGE_LOOP('',(#9964));
#3285=EDGE_LOOP('',(#9965));
#3286=EDGE_LOOP('',(#9966));
#3287=EDGE_LOOP('',(#9967));
#3288=EDGE_LOOP('',(#9968,#9969,#9970,#9971));
#3289=EDGE_LOOP('',(#9972,#9973,#9974,#9975));
#3290=EDGE_LOOP('',(#9976));
#3291=EDGE_LOOP('',(#9977));
#3292=EDGE_LOOP('',(#9978));
#3293=EDGE_LOOP('',(#9979));
#3294=EDGE_LOOP('',(#9980,#9981,#9982,#9983));
#3295=EDGE_LOOP('',(#9984,#9985,#9986,#9987));
#3296=EDGE_LOOP('',(#9988));
#3297=EDGE_LOOP('',(#9989));
#3298=EDGE_LOOP('',(#9990));
#3299=EDGE_LOOP('',(#9991));
#3300=EDGE_LOOP('',(#9992));
#3301=EDGE_LOOP('',(#9993,#9994,#9995,#9996));
#3302=EDGE_LOOP('',(#9997,#9998,#9999,#10000));
#3303=EDGE_LOOP('',(#10001,#10002,#10003,#10004));
#3304=EDGE_LOOP('',(#10005));
#3305=EDGE_LOOP('',(#10006));
#3306=EDGE_LOOP('',(#10007,#10008,#10009,#10010));
#3307=EDGE_LOOP('',(#10011,#10012,#10013,#10014));
#3308=EDGE_LOOP('',(#10015,#10016,#10017,#10018));
#3309=EDGE_LOOP('',(#10019));
#3310=EDGE_LOOP('',(#10020,#10021,#10022,#10023));
#3311=EDGE_LOOP('',(#10024,#10025,#10026,#10027));
#3312=EDGE_LOOP('',(#10028,#10029,#10030,#10031));
#3313=EDGE_LOOP('',(#10032,#10033,#10034,#10035));
#3314=EDGE_LOOP('',(#10036,#10037,#10038,#10039));
#3315=EDGE_LOOP('',(#10040,#10041,#10042,#10043));
#3316=EDGE_LOOP('',(#10044,#10045,#10046,#10047,#10048,#10049));
#3317=EDGE_LOOP('',(#10050,#10051,#10052,#10053,#10054,#10055));
#3318=EDGE_LOOP('',(#10056,#10057,#10058,#10059));
#3319=EDGE_LOOP('',(#10060,#10061,#10062,#10063));
#3320=EDGE_LOOP('',(#10064,#10065,#10066,#10067));
#3321=EDGE_LOOP('',(#10068,#10069,#10070,#10071));
#3322=EDGE_LOOP('',(#10072,#10073,#10074,#10075));
#3323=EDGE_LOOP('',(#10076));
#3324=EDGE_LOOP('',(#10077));
#3325=EDGE_LOOP('',(#10078));
#3326=EDGE_LOOP('',(#10079,#10080,#10081,#10082));
#3327=EDGE_LOOP('',(#10083,#10084,#10085,#10086));
#3328=EDGE_LOOP('',(#10087));
#3329=EDGE_LOOP('',(#10088));
#3330=EDGE_LOOP('',(#10089));
#3331=EDGE_LOOP('',(#10090,#10091,#10092,#10093));
#3332=EDGE_LOOP('',(#10094,#10095,#10096,#10097));
#3333=EDGE_LOOP('',(#10098,#10099,#10100,#10101));
#3334=EDGE_LOOP('',(#10102));
#3335=EDGE_LOOP('',(#10103));
#3336=EDGE_LOOP('',(#10104,#10105,#10106,#10107));
#3337=EDGE_LOOP('',(#10108));
#3338=EDGE_LOOP('',(#10109));
#3339=EDGE_LOOP('',(#10110,#10111,#10112,#10113));
#3340=EDGE_LOOP('',(#10114,#10115,#10116,#10117));
#3341=EDGE_LOOP('',(#10118,#10119,#10120,#10121));
#3342=EDGE_LOOP('',(#10122,#10123,#10124,#10125));
#3343=EDGE_LOOP('',(#10126,#10127,#10128,#10129));
#3344=EDGE_LOOP('',(#10130,#10131,#10132,#10133));
#3345=EDGE_LOOP('',(#10134,#10135,#10136,#10137));
#3346=EDGE_LOOP('',(#10138,#10139,#10140,#10141));
#3347=EDGE_LOOP('',(#10142));
#3348=EDGE_LOOP('',(#10143));
#3349=EDGE_LOOP('',(#10144));
#3350=EDGE_LOOP('',(#10145,#10146,#10147,#10148));
#3351=EDGE_LOOP('',(#10149));
#3352=EDGE_LOOP('',(#10150));
#3353=EDGE_LOOP('',(#10151));
#3354=EDGE_LOOP('',(#10152,#10153,#10154,#10155));
#3355=EDGE_LOOP('',(#10156));
#3356=EDGE_LOOP('',(#10157));
#3357=EDGE_LOOP('',(#10158,#10159,#10160,#10161));
#3358=EDGE_LOOP('',(#10162));
#3359=EDGE_LOOP('',(#10163));
#3360=EDGE_LOOP('',(#10164,#10165,#10166,#10167));
#3361=EDGE_LOOP('',(#10168,#10169,#10170,#10171));
#3362=EDGE_LOOP('',(#10172,#10173,#10174,#10175));
#3363=EDGE_LOOP('',(#10176,#10177,#10178,#10179));
#3364=EDGE_LOOP('',(#10180,#10181,#10182,#10183));
#3365=EDGE_LOOP('',(#10184,#10185,#10186,#10187));
#3366=EDGE_LOOP('',(#10188,#10189,#10190,#10191));
#3367=EDGE_LOOP('',(#10192,#10193,#10194,#10195));
#3368=EDGE_LOOP('',(#10196));
#3369=EDGE_LOOP('',(#10197));
#3370=EDGE_LOOP('',(#10198));
#3371=EDGE_LOOP('',(#10199,#10200,#10201,#10202));
#3372=EDGE_LOOP('',(#10203));
#3373=EDGE_LOOP('',(#10204));
#3374=EDGE_LOOP('',(#10205));
#3375=EDGE_LOOP('',(#10206,#10207));
#3376=EDGE_LOOP('',(#10208,#10209,#10210,#10211,#10212,#10213,#10214,#10215));
#3377=EDGE_LOOP('',(#10216,#10217,#10218));
#3378=EDGE_LOOP('',(#10219,#10220,#10221,#10222));
#3379=EDGE_LOOP('',(#10223,#10224,#10225,#10226));
#3380=EDGE_LOOP('',(#10227,#10228,#10229,#10230));
#3381=EDGE_LOOP('',(#10231));
#3382=EDGE_LOOP('',(#10232,#10233,#10234,#10235));
#3383=EDGE_LOOP('',(#10236));
#3384=EDGE_LOOP('',(#10237,#10238,#10239,#10240));
#3385=EDGE_LOOP('',(#10241));
#3386=EDGE_LOOP('',(#10242,#10243,#10244,#10245));
#3387=EDGE_LOOP('',(#10246,#10247,#10248,#10249));
#3388=EDGE_LOOP('',(#10250,#10251,#10252,#10253));
#3389=EDGE_LOOP('',(#10254,#10255,#10256,#10257));
#3390=EDGE_LOOP('',(#10258));
#3391=EDGE_LOOP('',(#10259,#10260,#10261,#10262));
#3392=EDGE_LOOP('',(#10263));
#3393=EDGE_LOOP('',(#10264,#10265,#10266,#10267));
#3394=EDGE_LOOP('',(#10268));
#3395=EDGE_LOOP('',(#10269));
#3396=EDGE_LOOP('',(#10270));
#3397=EDGE_LOOP('',(#10271));
#3398=EDGE_LOOP('',(#10272,#10273,#10274,#10275));
#3399=EDGE_LOOP('',(#10276,#10277,#10278,#10279));
#3400=EDGE_LOOP('',(#10280));
#3401=EDGE_LOOP('',(#10281));
#3402=EDGE_LOOP('',(#10282));
#3403=EDGE_LOOP('',(#10283));
#3404=EDGE_LOOP('',(#10284,#10285,#10286,#10287));
#3405=EDGE_LOOP('',(#10288,#10289,#10290,#10291));
#3406=EDGE_LOOP('',(#10292));
#3407=EDGE_LOOP('',(#10293));
#3408=EDGE_LOOP('',(#10294));
#3409=EDGE_LOOP('',(#10295));
#3410=EDGE_LOOP('',(#10296,#10297,#10298,#10299));
#3411=EDGE_LOOP('',(#10300,#10301,#10302,#10303));
#3412=EDGE_LOOP('',(#10304));
#3413=EDGE_LOOP('',(#10305));
#3414=EDGE_LOOP('',(#10306));
#3415=EDGE_LOOP('',(#10307));
#3416=EDGE_LOOP('',(#10308,#10309,#10310,#10311));
#3417=EDGE_LOOP('',(#10312,#10313,#10314,#10315));
#3418=EDGE_LOOP('',(#10316));
#3419=EDGE_LOOP('',(#10317));
#3420=EDGE_LOOP('',(#10318));
#3421=EDGE_LOOP('',(#10319));
#3422=EDGE_LOOP('',(#10320,#10321,#10322,#10323));
#3423=EDGE_LOOP('',(#10324,#10325,#10326,#10327));
#3424=EDGE_LOOP('',(#10328));
#3425=EDGE_LOOP('',(#10329));
#3426=EDGE_LOOP('',(#10330));
#3427=EDGE_LOOP('',(#10331));
#3428=EDGE_LOOP('',(#10332,#10333,#10334,#10335));
#3429=EDGE_LOOP('',(#10336,#10337,#10338,#10339));
#3430=EDGE_LOOP('',(#10340));
#3431=EDGE_LOOP('',(#10341));
#3432=EDGE_LOOP('',(#10342));
#3433=EDGE_LOOP('',(#10343));
#3434=EDGE_LOOP('',(#10344,#10345,#10346,#10347));
#3435=EDGE_LOOP('',(#10348,#10349,#10350,#10351));
#3436=EDGE_LOOP('',(#10352,#10353,#10354,#10355));
#3437=EDGE_LOOP('',(#10356,#10357,#10358,#10359));
#3438=EDGE_LOOP('',(#10360,#10361,#10362,#10363));
#3439=EDGE_LOOP('',(#10364));
#3440=EDGE_LOOP('',(#10365));
#3441=EDGE_LOOP('',(#10366));
#3442=EDGE_LOOP('',(#10367,#10368,#10369,#10370));
#3443=EDGE_LOOP('',(#10371,#10372,#10373,#10374));
#3444=EDGE_LOOP('',(#10375));
#3445=EDGE_LOOP('',(#10376));
#3446=EDGE_LOOP('',(#10377));
#3447=EDGE_LOOP('',(#10378,#10379,#10380,#10381));
#3448=EDGE_LOOP('',(#10382,#10383,#10384,#10385));
#3449=EDGE_LOOP('',(#10386,#10387,#10388,#10389));
#3450=EDGE_LOOP('',(#10390));
#3451=EDGE_LOOP('',(#10391));
#3452=EDGE_LOOP('',(#10392,#10393,#10394,#10395));
#3453=EDGE_LOOP('',(#10396));
#3454=EDGE_LOOP('',(#10397));
#3455=EDGE_LOOP('',(#10398,#10399,#10400,#10401));
#3456=EDGE_LOOP('',(#10402,#10403,#10404,#10405));
#3457=EDGE_LOOP('',(#10406,#10407,#10408,#10409));
#3458=EDGE_LOOP('',(#10410,#10411,#10412,#10413));
#3459=EDGE_LOOP('',(#10414,#10415,#10416,#10417));
#3460=EDGE_LOOP('',(#10418,#10419,#10420,#10421));
#3461=EDGE_LOOP('',(#10422,#10423,#10424,#10425));
#3462=EDGE_LOOP('',(#10426,#10427,#10428,#10429));
#3463=EDGE_LOOP('',(#10430));
#3464=EDGE_LOOP('',(#10431));
#3465=EDGE_LOOP('',(#10432));
#3466=EDGE_LOOP('',(#10433,#10434,#10435,#10436));
#3467=EDGE_LOOP('',(#10437));
#3468=EDGE_LOOP('',(#10438));
#3469=EDGE_LOOP('',(#10439));
#3470=EDGE_LOOP('',(#10440,#10441,#10442,#10443));
#3471=EDGE_LOOP('',(#10444));
#3472=EDGE_LOOP('',(#10445));
#3473=EDGE_LOOP('',(#10446,#10447,#10448,#10449));
#3474=EDGE_LOOP('',(#10450));
#3475=EDGE_LOOP('',(#10451));
#3476=EDGE_LOOP('',(#10452,#10453,#10454,#10455));
#3477=EDGE_LOOP('',(#10456,#10457,#10458,#10459));
#3478=EDGE_LOOP('',(#10460,#10461,#10462,#10463));
#3479=EDGE_LOOP('',(#10464,#10465,#10466,#10467));
#3480=EDGE_LOOP('',(#10468,#10469,#10470,#10471));
#3481=EDGE_LOOP('',(#10472,#10473,#10474,#10475));
#3482=EDGE_LOOP('',(#10476,#10477,#10478,#10479));
#3483=EDGE_LOOP('',(#10480,#10481,#10482,#10483));
#3484=EDGE_LOOP('',(#10484));
#3485=EDGE_LOOP('',(#10485));
#3486=EDGE_LOOP('',(#10486));
#3487=EDGE_LOOP('',(#10487,#10488,#10489,#10490));
#3488=EDGE_LOOP('',(#10491));
#3489=EDGE_LOOP('',(#10492));
#3490=EDGE_LOOP('',(#10493));
#3491=EDGE_LOOP('',(#10494,#10495));
#3492=EDGE_LOOP('',(#10496,#10497,#10498,#10499,#10500,#10501,#10502,#10503));
#3493=EDGE_LOOP('',(#10504,#10505,#10506));
#3494=EDGE_LOOP('',(#10507,#10508,#10509,#10510));
#3495=EDGE_LOOP('',(#10511,#10512,#10513,#10514));
#3496=EDGE_LOOP('',(#10515,#10516,#10517,#10518));
#3497=EDGE_LOOP('',(#10519));
#3498=EDGE_LOOP('',(#10520,#10521,#10522,#10523));
#3499=EDGE_LOOP('',(#10524));
#3500=EDGE_LOOP('',(#10525,#10526,#10527,#10528));
#3501=EDGE_LOOP('',(#10529));
#3502=EDGE_LOOP('',(#10530,#10531,#10532,#10533));
#3503=EDGE_LOOP('',(#10534,#10535,#10536,#10537));
#3504=EDGE_LOOP('',(#10538,#10539,#10540,#10541));
#3505=EDGE_LOOP('',(#10542,#10543,#10544,#10545));
#3506=EDGE_LOOP('',(#10546));
#3507=EDGE_LOOP('',(#10547,#10548,#10549,#10550));
#3508=EDGE_LOOP('',(#10551));
#3509=EDGE_LOOP('',(#10552,#10553,#10554,#10555));
#3510=EDGE_LOOP('',(#10556));
#3511=EDGE_LOOP('',(#10557));
#3512=EDGE_LOOP('',(#10558));
#3513=EDGE_LOOP('',(#10559));
#3514=EDGE_LOOP('',(#10560,#10561,#10562,#10563));
#3515=EDGE_LOOP('',(#10564,#10565,#10566,#10567));
#3516=EDGE_LOOP('',(#10568));
#3517=EDGE_LOOP('',(#10569));
#3518=EDGE_LOOP('',(#10570));
#3519=EDGE_LOOP('',(#10571));
#3520=EDGE_LOOP('',(#10572,#10573,#10574,#10575));
#3521=EDGE_LOOP('',(#10576,#10577,#10578,#10579));
#3522=EDGE_LOOP('',(#10580));
#3523=EDGE_LOOP('',(#10581));
#3524=EDGE_LOOP('',(#10582));
#3525=EDGE_LOOP('',(#10583));
#3526=EDGE_LOOP('',(#10584,#10585,#10586,#10587));
#3527=EDGE_LOOP('',(#10588,#10589,#10590,#10591));
#3528=EDGE_LOOP('',(#10592));
#3529=EDGE_LOOP('',(#10593));
#3530=EDGE_LOOP('',(#10594));
#3531=EDGE_LOOP('',(#10595));
#3532=EDGE_LOOP('',(#10596,#10597,#10598,#10599));
#3533=EDGE_LOOP('',(#10600,#10601,#10602,#10603));
#3534=EDGE_LOOP('',(#10604));
#3535=EDGE_LOOP('',(#10605));
#3536=EDGE_LOOP('',(#10606));
#3537=EDGE_LOOP('',(#10607));
#3538=EDGE_LOOP('',(#10608,#10609,#10610,#10611));
#3539=EDGE_LOOP('',(#10612,#10613,#10614,#10615));
#3540=EDGE_LOOP('',(#10616));
#3541=EDGE_LOOP('',(#10617));
#3542=EDGE_LOOP('',(#10618));
#3543=EDGE_LOOP('',(#10619));
#3544=EDGE_LOOP('',(#10620,#10621,#10622,#10623));
#3545=EDGE_LOOP('',(#10624,#10625,#10626,#10627));
#3546=EDGE_LOOP('',(#10628));
#3547=EDGE_LOOP('',(#10629));
#3548=EDGE_LOOP('',(#10630));
#3549=EDGE_LOOP('',(#10631));
#3550=EDGE_LOOP('',(#10632,#10633,#10634,#10635));
#3551=EDGE_LOOP('',(#10636,#10637,#10638,#10639));
#3552=EDGE_LOOP('',(#10640,#10641,#10642,#10643));
#3553=EDGE_LOOP('',(#10644,#10645,#10646,#10647));
#3554=EDGE_LOOP('',(#10648,#10649,#10650,#10651));
#3555=EDGE_LOOP('',(#10652));
#3556=EDGE_LOOP('',(#10653));
#3557=EDGE_LOOP('',(#10654,#10655,#10656,#10657));
#3558=EDGE_LOOP('',(#10658));
#3559=EDGE_LOOP('',(#10659));
#3560=EDGE_LOOP('',(#10660,#10661,#10662,#10663));
#3561=EDGE_LOOP('',(#10664));
#3562=EDGE_LOOP('',(#10665));
#3563=EDGE_LOOP('',(#10666,#10667,#10668,#10669));
#3564=EDGE_LOOP('',(#10670));
#3565=EDGE_LOOP('',(#10671));
#3566=EDGE_LOOP('',(#10672,#10673,#10674,#10675));
#3567=EDGE_LOOP('',(#10676));
#3568=EDGE_LOOP('',(#10677));
#3569=EDGE_LOOP('',(#10678,#10679,#10680,#10681));
#3570=EDGE_LOOP('',(#10682));
#3571=EDGE_LOOP('',(#10683));
#3572=EDGE_LOOP('',(#10684,#10685,#10686,#10687));
#3573=EDGE_LOOP('',(#10688,#10689,#10690,#10691));
#3574=EDGE_LOOP('',(#10692,#10693,#10694,#10695));
#3575=EDGE_LOOP('',(#10696,#10697,#10698,#10699));
#3576=EDGE_LOOP('',(#10700,#10701,#10702,#10703));
#3577=EDGE_LOOP('',(#10704,#10705,#10706,#10707));
#3578=EDGE_LOOP('',(#10708));
#3579=EDGE_LOOP('',(#10709));
#3580=EDGE_LOOP('',(#10710,#10711,#10712,#10713));
#3581=EDGE_LOOP('',(#10714,#10715,#10716,#10717));
#3582=EDGE_LOOP('',(#10718));
#3583=EDGE_LOOP('',(#10719));
#3584=EDGE_LOOP('',(#10720,#10721,#10722,#10723));
#3585=EDGE_LOOP('',(#10724,#10725,#10726,#10727));
#3586=EDGE_LOOP('',(#10728));
#3587=EDGE_LOOP('',(#10729,#10730,#10731,#10732));
#3588=EDGE_LOOP('',(#10733,#10734,#10735,#10736));
#3589=EDGE_LOOP('',(#10737,#10738,#10739,#10740));
#3590=EDGE_LOOP('',(#10741,#10742,#10743,#10744));
#3591=EDGE_LOOP('',(#10745,#10746,#10747,#10748));
#3592=EDGE_LOOP('',(#10749,#10750,#10751,#10752));
#3593=EDGE_LOOP('',(#10753,#10754,#10755,#10756,#10757,#10758));
#3594=EDGE_LOOP('',(#10759));
#3595=EDGE_LOOP('',(#10760,#10761,#10762,#10763,#10764,#10765));
#3596=EDGE_LOOP('',(#10766,#10767,#10768,#10769));
#3597=EDGE_LOOP('',(#10770,#10771,#10772,#10773));
#3598=EDGE_LOOP('',(#10774,#10775,#10776,#10777));
#3599=EDGE_LOOP('',(#10778,#10779,#10780,#10781));
#3600=EDGE_LOOP('',(#10782,#10783,#10784,#10785));
#3601=EDGE_LOOP('',(#10786,#10787,#10788,#10789));
#3602=EDGE_LOOP('',(#10790,#10791,#10792,#10793));
#3603=EDGE_LOOP('',(#10794,#10795,#10796,#10797));
#3604=EDGE_LOOP('',(#10798,#10799,#10800,#10801));
#3605=EDGE_LOOP('',(#10802,#10803,#10804,#10805));
#3606=EDGE_LOOP('',(#10806,#10807,#10808,#10809,#10810,#10811,#10812,#10813));
#3607=EDGE_LOOP('',(#10814));
#3608=EDGE_LOOP('',(#10815));
#3609=EDGE_LOOP('',(#10816));
#3610=EDGE_LOOP('',(#10817,#10818,#10819,#10820));
#3611=EDGE_LOOP('',(#10821,#10822,#10823,#10824));
#3612=EDGE_LOOP('',(#10825,#10826,#10827,#10828));
#3613=EDGE_LOOP('',(#10829,#10830,#10831,#10832,#10833,#10834,#10835,#10836));
#3614=EDGE_LOOP('',(#10837));
#3615=EDGE_LOOP('',(#10838));
#3616=EDGE_LOOP('',(#10839));
#3617=EDGE_LOOP('',(#10840,#10841,#10842,#10843));
#3618=EDGE_LOOP('',(#10844,#10845,#10846,#10847));
#3619=EDGE_LOOP('',(#10848));
#3620=EDGE_LOOP('',(#10849));
#3621=EDGE_LOOP('',(#10850));
#3622=EDGE_LOOP('',(#10851));
#3623=EDGE_LOOP('',(#10852,#10853,#10854,#10855));
#3624=EDGE_LOOP('',(#10856,#10857,#10858,#10859));
#3625=EDGE_LOOP('',(#10860));
#3626=EDGE_LOOP('',(#10861));
#3627=EDGE_LOOP('',(#10862));
#3628=EDGE_LOOP('',(#10863));
#3629=EDGE_LOOP('',(#10864,#10865,#10866,#10867));
#3630=EDGE_LOOP('',(#10868,#10869,#10870,#10871));
#3631=EDGE_LOOP('',(#10872));
#3632=EDGE_LOOP('',(#10873));
#3633=EDGE_LOOP('',(#10874));
#3634=EDGE_LOOP('',(#10875));
#3635=EDGE_LOOP('',(#10876,#10877,#10878,#10879));
#3636=EDGE_LOOP('',(#10880,#10881,#10882,#10883));
#3637=EDGE_LOOP('',(#10884,#10885,#10886,#10887));
#3638=EDGE_LOOP('',(#10888,#10889,#10890,#10891));
#3639=EDGE_LOOP('',(#10892,#10893,#10894,#10895));
#3640=EDGE_LOOP('',(#10896,#10897,#10898,#10899));
#3641=EDGE_LOOP('',(#10900,#10901,#10902,#10903));
#3642=EDGE_LOOP('',(#10904,#10905,#10906,#10907));
#3643=EDGE_LOOP('',(#10908,#10909,#10910,#10911,#10912,#10913,#10914,#10915));
#3644=EDGE_LOOP('',(#10916));
#3645=EDGE_LOOP('',(#10917));
#3646=EDGE_LOOP('',(#10918));
#3647=EDGE_LOOP('',(#10919,#10920,#10921,#10922));
#3648=EDGE_LOOP('',(#10923,#10924,#10925,#10926));
#3649=EDGE_LOOP('',(#10927,#10928,#10929,#10930));
#3650=EDGE_LOOP('',(#10931,#10932,#10933,#10934,#10935,#10936,#10937,#10938));
#3651=EDGE_LOOP('',(#10939));
#3652=EDGE_LOOP('',(#10940));
#3653=EDGE_LOOP('',(#10941));
#3654=EDGE_LOOP('',(#10942,#10943,#10944,#10945));
#3655=EDGE_LOOP('',(#10946,#10947,#10948,#10949));
#3656=EDGE_LOOP('',(#10950));
#3657=EDGE_LOOP('',(#10951));
#3658=EDGE_LOOP('',(#10952));
#3659=EDGE_LOOP('',(#10953));
#3660=EDGE_LOOP('',(#10954,#10955,#10956,#10957));
#3661=EDGE_LOOP('',(#10958,#10959,#10960,#10961));
#3662=EDGE_LOOP('',(#10962));
#3663=EDGE_LOOP('',(#10963));
#3664=EDGE_LOOP('',(#10964));
#3665=EDGE_LOOP('',(#10965));
#3666=EDGE_LOOP('',(#10966,#10967,#10968,#10969));
#3667=EDGE_LOOP('',(#10970,#10971,#10972,#10973));
#3668=EDGE_LOOP('',(#10974));
#3669=EDGE_LOOP('',(#10975));
#3670=EDGE_LOOP('',(#10976));
#3671=EDGE_LOOP('',(#10977));
#3672=EDGE_LOOP('',(#10978,#10979,#10980,#10981));
#3673=EDGE_LOOP('',(#10982));
#3674=EDGE_LOOP('',(#10983,#10984,#10985,#10986));
#3675=EDGE_LOOP('',(#10987));
#3676=EDGE_LOOP('',(#10988,#10989,#10990,#10991));
#3677=EDGE_LOOP('',(#10992));
#3678=EDGE_LOOP('',(#10993));
#3679=EDGE_LOOP('',(#10994));
#3680=EDGE_LOOP('',(#10995));
#3681=EDGE_LOOP('',(#10996,#10997,#10998,#10999));
#3682=EDGE_LOOP('',(#11000,#11001,#11002,#11003));
#3683=EDGE_LOOP('',(#11004));
#3684=EDGE_LOOP('',(#11005));
#3685=EDGE_LOOP('',(#11006));
#3686=EDGE_LOOP('',(#11007));
#3687=EDGE_LOOP('',(#11008,#11009,#11010,#11011));
#3688=EDGE_LOOP('',(#11012,#11013,#11014,#11015));
#3689=EDGE_LOOP('',(#11016));
#3690=EDGE_LOOP('',(#11017));
#3691=EDGE_LOOP('',(#11018));
#3692=EDGE_LOOP('',(#11019));
#3693=EDGE_LOOP('',(#11020,#11021,#11022,#11023));
#3694=EDGE_LOOP('',(#11024,#11025,#11026,#11027));
#3695=EDGE_LOOP('',(#11028));
#3696=EDGE_LOOP('',(#11029));
#3697=EDGE_LOOP('',(#11030));
#3698=EDGE_LOOP('',(#11031));
#3699=EDGE_LOOP('',(#11032,#11033,#11034,#11035));
#3700=EDGE_LOOP('',(#11036,#11037,#11038,#11039));
#3701=EDGE_LOOP('',(#11040));
#3702=EDGE_LOOP('',(#11041));
#3703=EDGE_LOOP('',(#11042));
#3704=EDGE_LOOP('',(#11043));
#3705=EDGE_LOOP('',(#11044,#11045,#11046,#11047));
#3706=EDGE_LOOP('',(#11048,#11049,#11050,#11051));
#3707=EDGE_LOOP('',(#11052));
#3708=EDGE_LOOP('',(#11053));
#3709=EDGE_LOOP('',(#11054));
#3710=EDGE_LOOP('',(#11055));
#3711=EDGE_LOOP('',(#11056,#11057,#11058,#11059));
#3712=EDGE_LOOP('',(#11060,#11061,#11062,#11063));
#3713=EDGE_LOOP('',(#11064));
#3714=EDGE_LOOP('',(#11065));
#3715=EDGE_LOOP('',(#11066));
#3716=EDGE_LOOP('',(#11067));
#3717=EDGE_LOOP('',(#11068,#11069,#11070,#11071));
#3718=EDGE_LOOP('',(#11072,#11073,#11074,#11075));
#3719=EDGE_LOOP('',(#11076));
#3720=EDGE_LOOP('',(#11077));
#3721=EDGE_LOOP('',(#11078));
#3722=EDGE_LOOP('',(#11079));
#3723=EDGE_LOOP('',(#11080));
#3724=EDGE_LOOP('',(#11081,#11082,#11083,#11084));
#3725=EDGE_LOOP('',(#11085,#11086,#11087,#11088));
#3726=EDGE_LOOP('',(#11089,#11090,#11091,#11092));
#3727=EDGE_LOOP('',(#11093));
#3728=EDGE_LOOP('',(#11094));
#3729=EDGE_LOOP('',(#11095,#11096,#11097,#11098));
#3730=EDGE_LOOP('',(#11099,#11100,#11101,#11102));
#3731=EDGE_LOOP('',(#11103,#11104,#11105,#11106));
#3732=EDGE_LOOP('',(#11107));
#3733=EDGE_LOOP('',(#11108,#11109,#11110,#11111));
#3734=EDGE_LOOP('',(#11112,#11113,#11114,#11115));
#3735=EDGE_LOOP('',(#11116,#11117,#11118,#11119));
#3736=EDGE_LOOP('',(#11120,#11121,#11122,#11123));
#3737=EDGE_LOOP('',(#11124,#11125,#11126,#11127));
#3738=EDGE_LOOP('',(#11128,#11129,#11130,#11131));
#3739=EDGE_LOOP('',(#11132,#11133,#11134,#11135,#11136,#11137));
#3740=EDGE_LOOP('',(#11138,#11139,#11140,#11141,#11142,#11143));
#3741=EDGE_LOOP('',(#11144,#11145,#11146,#11147));
#3742=EDGE_LOOP('',(#11148,#11149,#11150,#11151));
#3743=EDGE_LOOP('',(#11152,#11153,#11154,#11155));
#3744=EDGE_LOOP('',(#11156,#11157,#11158,#11159));
#3745=EDGE_LOOP('',(#11160,#11161,#11162,#11163));
#3746=EDGE_LOOP('',(#11164,#11165,#11166,#11167));
#3747=EDGE_LOOP('',(#11168,#11169,#11170,#11171));
#3748=EDGE_LOOP('',(#11172,#11173,#11174,#11175));
#3749=EDGE_LOOP('',(#11176,#11177,#11178,#11179,#11180,#11181,#11182,#11183));
#3750=EDGE_LOOP('',(#11184));
#3751=EDGE_LOOP('',(#11185));
#3752=EDGE_LOOP('',(#11186));
#3753=EDGE_LOOP('',(#11187));
#3754=EDGE_LOOP('',(#11188));
#3755=EDGE_LOOP('',(#11189));
#3756=EDGE_LOOP('',(#11190));
#3757=EDGE_LOOP('',(#11191,#11192,#11193,#11194));
#3758=EDGE_LOOP('',(#11195,#11196,#11197,#11198));
#3759=EDGE_LOOP('',(#11199,#11200,#11201,#11202));
#3760=EDGE_LOOP('',(#11203,#11204,#11205,#11206));
#3761=EDGE_LOOP('',(#11207,#11208,#11209,#11210));
#3762=EDGE_LOOP('',(#11211,#11212,#11213,#11214));
#3763=EDGE_LOOP('',(#11215,#11216,#11217,#11218));
#3764=EDGE_LOOP('',(#11219,#11220,#11221,#11222,#11223,#11224,#11225,#11226));
#3765=EDGE_LOOP('',(#11227));
#3766=EDGE_LOOP('',(#11228));
#3767=EDGE_LOOP('',(#11229));
#3768=EDGE_LOOP('',(#11230));
#3769=EDGE_LOOP('',(#11231));
#3770=EDGE_LOOP('',(#11232));
#3771=EDGE_LOOP('',(#11233));
#3772=EDGE_LOOP('',(#11234,#11235,#11236,#11237));
#3773=EDGE_LOOP('',(#11238,#11239,#11240,#11241));
#3774=EDGE_LOOP('',(#11242));
#3775=EDGE_LOOP('',(#11243));
#3776=EDGE_LOOP('',(#11244));
#3777=EDGE_LOOP('',(#11245));
#3778=EDGE_LOOP('',(#11246,#11247,#11248,#11249));
#3779=EDGE_LOOP('',(#11250,#11251,#11252,#11253));
#3780=EDGE_LOOP('',(#11254));
#3781=EDGE_LOOP('',(#11255));
#3782=EDGE_LOOP('',(#11256));
#3783=EDGE_LOOP('',(#11257));
#3784=EDGE_LOOP('',(#11258,#11259,#11260,#11261));
#3785=EDGE_LOOP('',(#11262,#11263,#11264,#11265));
#3786=EDGE_LOOP('',(#11266,#11267,#11268,#11269));
#3787=EDGE_LOOP('',(#11270,#11271,#11272,#11273));
#3788=EDGE_LOOP('',(#11274,#11275,#11276,#11277));
#3789=EDGE_LOOP('',(#11278,#11279,#11280,#11281));
#3790=EDGE_LOOP('',(#11282));
#3791=EDGE_LOOP('',(#11283));
#3792=EDGE_LOOP('',(#11284));
#3793=EDGE_LOOP('',(#11285));
#3794=EDGE_LOOP('',(#11286));
#3795=EDGE_LOOP('',(#11287));
#3796=EDGE_LOOP('',(#11288));
#3797=EDGE_LOOP('',(#11289));
#3798=EDGE_LOOP('',(#11290));
#3799=EDGE_LOOP('',(#11291));
#3800=EDGE_LOOP('',(#11292));
#3801=EDGE_LOOP('',(#11293));
#3802=EDGE_LOOP('',(#11294));
#3803=EDGE_LOOP('',(#11295));
#3804=EDGE_LOOP('',(#11296,#11297,#11298,#11299));
#3805=EDGE_LOOP('',(#11300));
#3806=EDGE_LOOP('',(#11301,#11302,#11303,#11304));
#3807=EDGE_LOOP('',(#11305));
#3808=EDGE_LOOP('',(#11306));
#3809=EDGE_LOOP('',(#11307));
#3810=EDGE_LOOP('',(#11308,#11309,#11310,#11311));
#3811=EDGE_LOOP('',(#11312));
#3812=EDGE_LOOP('',(#11313,#11314,#11315,#11316));
#3813=EDGE_LOOP('',(#11317));
#3814=EDGE_LOOP('',(#11318));
#3815=EDGE_LOOP('',(#11319));
#3816=EDGE_LOOP('',(#11320,#11321,#11322,#11323));
#3817=EDGE_LOOP('',(#11324));
#3818=EDGE_LOOP('',(#11325,#11326,#11327,#11328));
#3819=EDGE_LOOP('',(#11329));
#3820=EDGE_LOOP('',(#11330));
#3821=EDGE_LOOP('',(#11331));
#3822=EDGE_LOOP('',(#11332,#11333,#11334,#11335));
#3823=EDGE_LOOP('',(#11336));
#3824=EDGE_LOOP('',(#11337,#11338,#11339,#11340));
#3825=EDGE_LOOP('',(#11341));
#3826=EDGE_LOOP('',(#11342,#11343,#11344,#11345));
#3827=EDGE_LOOP('',(#11346,#11347,#11348,#11349));
#3828=EDGE_LOOP('',(#11350,#11351,#11352,#11353));
#3829=EDGE_LOOP('',(#11354,#11355,#11356,#11357));
#3830=EDGE_LOOP('',(#11358,#11359,#11360,#11361));
#3831=EDGE_LOOP('',(#11362,#11363,#11364,#11365));
#3832=EDGE_LOOP('',(#11366));
#3833=EDGE_LOOP('',(#11367));
#3834=EDGE_LOOP('',(#11368));
#3835=EDGE_LOOP('',(#11369));
#3836=EDGE_LOOP('',(#11370));
#3837=EDGE_LOOP('',(#11371));
#3838=EDGE_LOOP('',(#11372));
#3839=EDGE_LOOP('',(#11373));
#3840=EDGE_LOOP('',(#11374));
#3841=EDGE_LOOP('',(#11375));
#3842=EDGE_LOOP('',(#11376));
#3843=EDGE_LOOP('',(#11377));
#3844=EDGE_LOOP('',(#11378));
#3845=EDGE_LOOP('',(#11379));
#3846=EDGE_LOOP('',(#11380,#11381,#11382,#11383));
#3847=EDGE_LOOP('',(#11384));
#3848=EDGE_LOOP('',(#11385,#11386,#11387,#11388));
#3849=EDGE_LOOP('',(#11389));
#3850=EDGE_LOOP('',(#11390));
#3851=EDGE_LOOP('',(#11391));
#3852=EDGE_LOOP('',(#11392,#11393,#11394,#11395));
#3853=EDGE_LOOP('',(#11396));
#3854=EDGE_LOOP('',(#11397,#11398,#11399,#11400));
#3855=EDGE_LOOP('',(#11401));
#3856=EDGE_LOOP('',(#11402));
#3857=EDGE_LOOP('',(#11403));
#3858=EDGE_LOOP('',(#11404,#11405,#11406,#11407));
#3859=EDGE_LOOP('',(#11408));
#3860=EDGE_LOOP('',(#11409,#11410,#11411,#11412));
#3861=EDGE_LOOP('',(#11413));
#3862=EDGE_LOOP('',(#11414));
#3863=EDGE_LOOP('',(#11415));
#3864=EDGE_LOOP('',(#11416,#11417,#11418,#11419));
#3865=EDGE_LOOP('',(#11420));
#3866=EDGE_LOOP('',(#11421,#11422,#11423,#11424));
#3867=EDGE_LOOP('',(#11425));
#3868=EDGE_LOOP('',(#11426,#11427,#11428,#11429));
#3869=EDGE_LOOP('',(#11430,#11431,#11432,#11433));
#3870=EDGE_LOOP('',(#11434,#11435,#11436,#11437));
#3871=EDGE_LOOP('',(#11438,#11439,#11440,#11441));
#3872=EDGE_LOOP('',(#11442,#11443,#11444,#11445));
#3873=EDGE_LOOP('',(#11446,#11447,#11448,#11449));
#3874=EDGE_LOOP('',(#11450,#11451,#11452,#11453));
#3875=EDGE_LOOP('',(#11454,#11455,#11456,#11457));
#3876=EDGE_LOOP('',(#11458,#11459,#11460,#11461,#11462,#11463,#11464,#11465));
#3877=EDGE_LOOP('',(#11466));
#3878=EDGE_LOOP('',(#11467));
#3879=EDGE_LOOP('',(#11468));
#3880=EDGE_LOOP('',(#11469));
#3881=EDGE_LOOP('',(#11470));
#3882=EDGE_LOOP('',(#11471));
#3883=EDGE_LOOP('',(#11472));
#3884=EDGE_LOOP('',(#11473,#11474,#11475,#11476));
#3885=EDGE_LOOP('',(#11477,#11478,#11479,#11480));
#3886=EDGE_LOOP('',(#11481,#11482,#11483,#11484));
#3887=EDGE_LOOP('',(#11485,#11486,#11487,#11488));
#3888=EDGE_LOOP('',(#11489,#11490,#11491,#11492));
#3889=EDGE_LOOP('',(#11493,#11494,#11495,#11496));
#3890=EDGE_LOOP('',(#11497,#11498,#11499,#11500));
#3891=EDGE_LOOP('',(#11501,#11502,#11503,#11504,#11505,#11506,#11507,#11508));
#3892=EDGE_LOOP('',(#11509));
#3893=EDGE_LOOP('',(#11510));
#3894=EDGE_LOOP('',(#11511));
#3895=EDGE_LOOP('',(#11512));
#3896=EDGE_LOOP('',(#11513));
#3897=EDGE_LOOP('',(#11514));
#3898=EDGE_LOOP('',(#11515));
#3899=EDGE_LOOP('',(#11516,#11517,#11518,#11519));
#3900=EDGE_LOOP('',(#11520,#11521,#11522,#11523));
#3901=EDGE_LOOP('',(#11524));
#3902=EDGE_LOOP('',(#11525));
#3903=EDGE_LOOP('',(#11526));
#3904=EDGE_LOOP('',(#11527));
#3905=EDGE_LOOP('',(#11528,#11529,#11530,#11531));
#3906=EDGE_LOOP('',(#11532,#11533,#11534,#11535));
#3907=EDGE_LOOP('',(#11536));
#3908=EDGE_LOOP('',(#11537));
#3909=EDGE_LOOP('',(#11538));
#3910=EDGE_LOOP('',(#11539));
#3911=EDGE_LOOP('',(#11540,#11541,#11542,#11543));
#3912=EDGE_LOOP('',(#11544,#11545,#11546,#11547));
#3913=EDGE_LOOP('',(#11548,#11549,#11550,#11551));
#3914=EDGE_LOOP('',(#11552,#11553,#11554,#11555));
#3915=EDGE_LOOP('',(#11556,#11557,#11558,#11559));
#3916=EDGE_LOOP('',(#11560,#11561,#11562,#11563));
#3917=EDGE_LOOP('',(#11564));
#3918=EDGE_LOOP('',(#11565));
#3919=EDGE_LOOP('',(#11566));
#3920=EDGE_LOOP('',(#11567));
#3921=EDGE_LOOP('',(#11568));
#3922=EDGE_LOOP('',(#11569));
#3923=EDGE_LOOP('',(#11570));
#3924=EDGE_LOOP('',(#11571));
#3925=EDGE_LOOP('',(#11572));
#3926=EDGE_LOOP('',(#11573));
#3927=EDGE_LOOP('',(#11574));
#3928=EDGE_LOOP('',(#11575));
#3929=EDGE_LOOP('',(#11576));
#3930=EDGE_LOOP('',(#11577));
#3931=EDGE_LOOP('',(#11578,#11579,#11580,#11581));
#3932=EDGE_LOOP('',(#11582));
#3933=EDGE_LOOP('',(#11583,#11584,#11585,#11586));
#3934=EDGE_LOOP('',(#11587));
#3935=EDGE_LOOP('',(#11588));
#3936=EDGE_LOOP('',(#11589));
#3937=EDGE_LOOP('',(#11590,#11591,#11592,#11593));
#3938=EDGE_LOOP('',(#11594));
#3939=EDGE_LOOP('',(#11595,#11596,#11597,#11598));
#3940=EDGE_LOOP('',(#11599));
#3941=EDGE_LOOP('',(#11600));
#3942=EDGE_LOOP('',(#11601));
#3943=EDGE_LOOP('',(#11602,#11603,#11604,#11605));
#3944=EDGE_LOOP('',(#11606));
#3945=EDGE_LOOP('',(#11607,#11608,#11609,#11610));
#3946=EDGE_LOOP('',(#11611));
#3947=EDGE_LOOP('',(#11612));
#3948=EDGE_LOOP('',(#11613));
#3949=EDGE_LOOP('',(#11614,#11615,#11616,#11617));
#3950=EDGE_LOOP('',(#11618));
#3951=EDGE_LOOP('',(#11619,#11620,#11621,#11622));
#3952=EDGE_LOOP('',(#11623));
#3953=EDGE_LOOP('',(#11624,#11625,#11626,#11627));
#3954=EDGE_LOOP('',(#11628,#11629,#11630,#11631));
#3955=EDGE_LOOP('',(#11632,#11633,#11634,#11635));
#3956=EDGE_LOOP('',(#11636,#11637,#11638,#11639));
#3957=EDGE_LOOP('',(#11640,#11641,#11642,#11643));
#3958=EDGE_LOOP('',(#11644,#11645,#11646,#11647));
#3959=EDGE_LOOP('',(#11648));
#3960=EDGE_LOOP('',(#11649));
#3961=EDGE_LOOP('',(#11650));
#3962=EDGE_LOOP('',(#11651));
#3963=EDGE_LOOP('',(#11652));
#3964=EDGE_LOOP('',(#11653));
#3965=EDGE_LOOP('',(#11654));
#3966=EDGE_LOOP('',(#11655));
#3967=EDGE_LOOP('',(#11656));
#3968=EDGE_LOOP('',(#11657));
#3969=EDGE_LOOP('',(#11658));
#3970=EDGE_LOOP('',(#11659));
#3971=EDGE_LOOP('',(#11660));
#3972=EDGE_LOOP('',(#11661));
#3973=EDGE_LOOP('',(#11662,#11663,#11664,#11665));
#3974=EDGE_LOOP('',(#11666));
#3975=EDGE_LOOP('',(#11667,#11668,#11669,#11670));
#3976=EDGE_LOOP('',(#11671));
#3977=EDGE_LOOP('',(#11672));
#3978=EDGE_LOOP('',(#11673));
#3979=EDGE_LOOP('',(#11674,#11675,#11676,#11677));
#3980=EDGE_LOOP('',(#11678));
#3981=EDGE_LOOP('',(#11679,#11680,#11681,#11682));
#3982=EDGE_LOOP('',(#11683));
#3983=EDGE_LOOP('',(#11684));
#3984=EDGE_LOOP('',(#11685));
#3985=EDGE_LOOP('',(#11686,#11687,#11688,#11689));
#3986=EDGE_LOOP('',(#11690));
#3987=EDGE_LOOP('',(#11691,#11692,#11693,#11694));
#3988=EDGE_LOOP('',(#11695));
#3989=EDGE_LOOP('',(#11696));
#3990=EDGE_LOOP('',(#11697));
#3991=EDGE_LOOP('',(#11698,#11699,#11700,#11701));
#3992=EDGE_LOOP('',(#11702));
#3993=EDGE_LOOP('',(#11703,#11704,#11705,#11706));
#3994=EDGE_LOOP('',(#11707));
#3995=EDGE_LOOP('',(#11708,#11709,#11710,#11711,#11712,#11713));
#3996=EDGE_LOOP('',(#11714,#11715,#11716,#11717,#11718));
#3997=EDGE_LOOP('',(#11719,#11720,#11721,#11722));
#3998=EDGE_LOOP('',(#11723,#11724,#11725,#11726));
#3999=EDGE_LOOP('',(#11727));
#4000=EDGE_LOOP('',(#11728));
#4001=EDGE_LOOP('',(#11729,#11730,#11731,#11732,#11733));
#4002=EDGE_LOOP('',(#11734));
#4003=EDGE_LOOP('',(#11735));
#4004=EDGE_LOOP('',(#11736,#11737,#11738,#11739));
#4005=EDGE_LOOP('',(#11740,#11741,#11742,#11743,#11744,#11745));
#4006=EDGE_LOOP('',(#11746,#11747,#11748,#11749,#11750));
#4007=EDGE_LOOP('',(#11751));
#4008=EDGE_LOOP('',(#11752));
#4009=EDGE_LOOP('',(#11753,#11754,#11755,#11756));
#4010=EDGE_LOOP('',(#11757,#11758,#11759,#11760));
#4011=EDGE_LOOP('',(#11761,#11762,#11763,#11764));
#4012=EDGE_LOOP('',(#11765));
#4013=EDGE_LOOP('',(#11766));
#4014=EDGE_LOOP('',(#11767,#11768,#11769,#11770,#11771));
#4015=EDGE_LOOP('',(#11772,#11773));
#4016=EDGE_LOOP('',(#11774,#11775));
#4017=EDGE_LOOP('',(#11776,#11777));
#4018=EDGE_LOOP('',(#11778,#11779));
#4019=EDGE_LOOP('',(#11780,#11781));
#4020=EDGE_LOOP('',(#11782,#11783));
#4021=EDGE_LOOP('',(#11784,#11785));
#4022=EDGE_LOOP('',(#11786,#11787,#11788,#11789));
#4023=EDGE_LOOP('',(#11790,#11791,#11792,#11793));
#4024=EDGE_LOOP('',(#11794,#11795,#11796,#11797));
#4025=EDGE_LOOP('',(#11798,#11799,#11800,#11801));
#4026=EDGE_LOOP('',(#11802,#11803,#11804,#11805));
#4027=EDGE_LOOP('',(#11806,#11807,#11808,#11809));
#4028=EDGE_LOOP('',(#11810,#11811,#11812,#11813));
#4029=EDGE_LOOP('',(#11814,#11815,#11816,#11817));
#4030=EDGE_LOOP('',(#11818,#11819,#11820,#11821));
#4031=EDGE_LOOP('',(#11822,#11823,#11824,#11825));
#4032=EDGE_LOOP('',(#11826,#11827,#11828,#11829));
#4033=EDGE_LOOP('',(#11830,#11831,#11832,#11833));
#4034=EDGE_LOOP('',(#11834,#11835,#11836,#11837));
#4035=EDGE_LOOP('',(#11838,#11839,#11840,#11841));
#4036=EDGE_LOOP('',(#11842,#11843,#11844,#11845));
#4037=EDGE_LOOP('',(#11846,#11847,#11848,#11849));
#4038=EDGE_LOOP('',(#11850,#11851,#11852,#11853));
#4039=EDGE_LOOP('',(#11854,#11855,#11856,#11857));
#4040=EDGE_LOOP('',(#11858,#11859,#11860,#11861));
#4041=EDGE_LOOP('',(#11862,#11863,#11864,#11865));
#4042=EDGE_LOOP('',(#11866,#11867,#11868,#11869));
#4043=EDGE_LOOP('',(#11870,#11871,#11872,#11873));
#4044=EDGE_LOOP('',(#11874,#11875,#11876,#11877));
#4045=EDGE_LOOP('',(#11878,#11879,#11880,#11881));
#4046=EDGE_LOOP('',(#11882,#11883,#11884,#11885));
#4047=EDGE_LOOP('',(#11886,#11887,#11888,#11889));
#4048=EDGE_LOOP('',(#11890,#11891,#11892,#11893));
#4049=EDGE_LOOP('',(#11894,#11895,#11896,#11897));
#4050=EDGE_LOOP('',(#11898,#11899,#11900,#11901));
#4051=EDGE_LOOP('',(#11902,#11903,#11904,#11905));
#4052=EDGE_LOOP('',(#11906,#11907,#11908,#11909));
#4053=EDGE_LOOP('',(#11910,#11911,#11912,#11913));
#4054=EDGE_LOOP('',(#11914,#11915,#11916,#11917));
#4055=EDGE_LOOP('',(#11918,#11919,#11920,#11921));
#4056=EDGE_LOOP('',(#11922,#11923,#11924,#11925));
#4057=EDGE_LOOP('',(#11926,#11927,#11928,#11929));
#4058=EDGE_LOOP('',(#11930,#11931,#11932,#11933));
#4059=EDGE_LOOP('',(#11934,#11935,#11936,#11937));
#4060=EDGE_LOOP('',(#11938,#11939,#11940,#11941));
#4061=EDGE_LOOP('',(#11942,#11943,#11944,#11945));
#4062=EDGE_LOOP('',(#11946,#11947,#11948,#11949));
#4063=EDGE_LOOP('',(#11950,#11951,#11952,#11953));
#4064=EDGE_LOOP('',(#11954));
#4065=EDGE_LOOP('',(#11955));
#4066=EDGE_LOOP('',(#11956,#11957,#11958,#11959));
#4067=EDGE_LOOP('',(#11960));
#4068=EDGE_LOOP('',(#11961));
#4069=EDGE_LOOP('',(#11962,#11963,#11964,#11965));
#4070=EDGE_LOOP('',(#11966));
#4071=EDGE_LOOP('',(#11967));
#4072=EDGE_LOOP('',(#11968,#11969,#11970,#11971));
#4073=EDGE_LOOP('',(#11972));
#4074=EDGE_LOOP('',(#11973));
#4075=EDGE_LOOP('',(#11974,#11975,#11976,#11977));
#4076=EDGE_LOOP('',(#11978));
#4077=EDGE_LOOP('',(#11979));
#4078=EDGE_LOOP('',(#11980));
#4079=EDGE_LOOP('',(#11981));
#4080=EDGE_LOOP('',(#11982,#11983,#11984,#11985));
#4081=EDGE_LOOP('',(#11986,#11987,#11988,#11989));
#4082=EDGE_LOOP('',(#11990));
#4083=EDGE_LOOP('',(#11991));
#4084=EDGE_LOOP('',(#11992));
#4085=EDGE_LOOP('',(#11993));
#4086=EDGE_LOOP('',(#11994,#11995,#11996,#11997));
#4087=EDGE_LOOP('',(#11998,#11999,#12000,#12001));
#4088=EDGE_LOOP('',(#12002,#12003,#12004,#12005));
#4089=EDGE_LOOP('',(#12006));
#4090=EDGE_LOOP('',(#12007));
#4091=EDGE_LOOP('',(#12008,#12009,#12010,#12011));
#4092=EDGE_LOOP('',(#12012,#12013,#12014,#12015));
#4093=EDGE_LOOP('',(#12016));
#4094=EDGE_LOOP('',(#12017));
#4095=EDGE_LOOP('',(#12018));
#4096=EDGE_LOOP('',(#12019));
#4097=EDGE_LOOP('',(#12020,#12021,#12022,#12023));
#4098=EDGE_LOOP('',(#12024,#12025,#12026,#12027));
#4099=EDGE_LOOP('',(#12028));
#4100=EDGE_LOOP('',(#12029));
#4101=EDGE_LOOP('',(#12030));
#4102=EDGE_LOOP('',(#12031));
#4103=EDGE_LOOP('',(#12032,#12033,#12034,#12035));
#4104=EDGE_LOOP('',(#12036,#12037,#12038,#12039));
#4105=EDGE_LOOP('',(#12040));
#4106=EDGE_LOOP('',(#12041));
#4107=EDGE_LOOP('',(#12042));
#4108=EDGE_LOOP('',(#12043));
#4109=EDGE_LOOP('',(#12044,#12045,#12046,#12047));
#4110=EDGE_LOOP('',(#12048,#12049,#12050,#12051));
#4111=EDGE_LOOP('',(#12052));
#4112=EDGE_LOOP('',(#12053));
#4113=EDGE_LOOP('',(#12054));
#4114=EDGE_LOOP('',(#12055));
#4115=EDGE_LOOP('',(#12056,#12057,#12058,#12059));
#4116=EDGE_LOOP('',(#12060));
#4117=EDGE_LOOP('',(#12061,#12062,#12063,#12064));
#4118=EDGE_LOOP('',(#12065,#12066,#12067,#12068));
#4119=EDGE_LOOP('',(#12069));
#4120=EDGE_LOOP('',(#12070));
#4121=EDGE_LOOP('',(#12071));
#4122=EDGE_LOOP('',(#12072));
#4123=EDGE_LOOP('',(#12073));
#4124=LINE('',#20981,#4864);
#4125=LINE('',#20987,#4865);
#4126=LINE('',#20993,#4866);
#4127=LINE('',#20999,#4867);
#4128=LINE('',#21005,#4868);
#4129=LINE('',#21011,#4869);
#4130=LINE('',#21017,#4870);
#4131=LINE('',#21023,#4871);
#4132=LINE('',#21028,#4872);
#4133=LINE('',#21030,#4873);
#4134=LINE('',#21032,#4874);
#4135=LINE('',#21033,#4875);
#4136=LINE('',#21036,#4876);
#4137=LINE('',#21038,#4877);
#4138=LINE('',#21039,#4878);
#4139=LINE('',#21042,#4879);
#4140=LINE('',#21044,#4880);
#4141=LINE('',#21045,#4881);
#4142=LINE('',#21047,#4882);
#4143=LINE('',#21048,#4883);
#4144=LINE('',#21055,#4884);
#4145=LINE('',#21057,#4885);
#4146=LINE('',#21059,#4886);
#4147=LINE('',#21060,#4887);
#4148=LINE('',#21063,#4888);
#4149=LINE('',#21065,#4889);
#4150=LINE('',#21066,#4890);
#4151=LINE('',#21069,#4891);
#4152=LINE('',#21071,#4892);
#4153=LINE('',#21072,#4893);
#4154=LINE('',#21074,#4894);
#4155=LINE('',#21075,#4895);
#4156=LINE('',#21082,#4896);
#4157=LINE('',#21084,#4897);
#4158=LINE('',#21086,#4898);
#4159=LINE('',#21087,#4899);
#4160=LINE('',#21090,#4900);
#4161=LINE('',#21092,#4901);
#4162=LINE('',#21093,#4902);
#4163=LINE('',#21096,#4903);
#4164=LINE('',#21098,#4904);
#4165=LINE('',#21099,#4905);
#4166=LINE('',#21101,#4906);
#4167=LINE('',#21102,#4907);
#4168=LINE('',#21110,#4908);
#4169=LINE('',#21116,#4909);
#4170=LINE('',#21122,#4910);
#4171=LINE('',#21128,#4911);
#4172=LINE('',#21134,#4912);
#4173=LINE('',#21140,#4913);
#4174=LINE('',#21146,#4914);
#4175=LINE('',#21152,#4915);
#4176=LINE('',#21158,#4916);
#4177=LINE('',#21163,#4917);
#4178=LINE('',#21165,#4918);
#4179=LINE('',#21167,#4919);
#4180=LINE('',#21168,#4920);
#4181=LINE('',#21172,#4921);
#4182=LINE('',#21174,#4922);
#4183=LINE('',#21176,#4923);
#4184=LINE('',#21177,#4924);
#4185=LINE('',#21181,#4925);
#4186=LINE('',#21182,#4926);
#4187=LINE('',#21183,#4927);
#4188=LINE('',#21187,#4928);
#4189=LINE('',#21188,#4929);
#4190=LINE('',#21189,#4930);
#4191=LINE('',#21192,#4931);
#4192=LINE('',#21194,#4932);
#4193=LINE('',#21195,#4933);
#4194=LINE('',#21196,#4934);
#4195=LINE('',#21201,#4935);
#4196=LINE('',#21202,#4936);
#4197=LINE('',#21210,#4937);
#4198=LINE('',#21213,#4938);
#4199=LINE('',#21217,#4939);
#4200=LINE('',#21221,#4940);
#4201=LINE('',#21222,#4941);
#4202=LINE('',#21224,#4942);
#4203=LINE('',#21225,#4943);
#4204=LINE('',#21233,#4944);
#4205=LINE('',#21239,#4945);
#4206=LINE('',#21245,#4946);
#4207=LINE('',#21251,#4947);
#4208=LINE('',#21257,#4948);
#4209=LINE('',#21264,#4949);
#4210=LINE('',#21270,#4950);
#4211=LINE('',#21279,#4951);
#4212=LINE('',#21285,#4952);
#4213=LINE('',#21291,#4953);
#4214=LINE('',#21297,#4954);
#4215=LINE('',#21303,#4955);
#4216=LINE('',#21311,#4956);
#4217=LINE('',#21316,#4957);
#4218=LINE('',#21325,#4958);
#4219=LINE('',#21331,#4959);
#4220=LINE('',#21337,#4960);
#4221=LINE('',#21343,#4961);
#4222=LINE('',#21349,#4962);
#4223=LINE('',#21355,#4963);
#4224=LINE('',#21361,#4964);
#4225=LINE('',#21367,#4965);
#4226=LINE('',#21373,#4966);
#4227=LINE('',#21378,#4967);
#4228=LINE('',#21380,#4968);
#4229=LINE('',#21382,#4969);
#4230=LINE('',#21383,#4970);
#4231=LINE('',#21387,#4971);
#4232=LINE('',#21389,#4972);
#4233=LINE('',#21391,#4973);
#4234=LINE('',#21392,#4974);
#4235=LINE('',#21396,#4975);
#4236=LINE('',#21397,#4976);
#4237=LINE('',#21398,#4977);
#4238=LINE('',#21402,#4978);
#4239=LINE('',#21403,#4979);
#4240=LINE('',#21404,#4980);
#4241=LINE('',#21407,#4981);
#4242=LINE('',#21409,#4982);
#4243=LINE('',#21410,#4983);
#4244=LINE('',#21411,#4984);
#4245=LINE('',#21414,#4985);
#4246=LINE('',#21415,#4986);
#4247=LINE('',#21422,#4987);
#4248=LINE('',#21426,#4988);
#4249=LINE('',#21430,#4989);
#4250=LINE('',#21431,#4990);
#4251=LINE('',#21433,#4991);
#4252=LINE('',#21434,#4992);
#4253=LINE('',#21442,#4993);
#4254=LINE('',#21448,#4994);
#4255=LINE('',#21454,#4995);
#4256=LINE('',#21460,#4996);
#4257=LINE('',#21466,#4997);
#4258=LINE('',#21473,#4998);
#4259=LINE('',#21479,#4999);
#4260=LINE('',#21488,#5000);
#4261=LINE('',#21494,#5001);
#4262=LINE('',#21500,#5002);
#4263=LINE('',#21506,#5003);
#4264=LINE('',#21512,#5004);
#4265=LINE('',#21520,#5005);
#4266=LINE('',#21525,#5006);
#4267=LINE('',#21534,#5007);
#4268=LINE('',#21543,#5008);
#4269=LINE('',#21552,#5009);
#4270=LINE('',#21559,#5010);
#4271=LINE('',#21566,#5011);
#4272=LINE('',#21575,#5012);
#4273=LINE('',#21581,#5013);
#4274=LINE('',#21590,#5014);
#4275=LINE('',#21596,#5015);
#4276=LINE('',#21605,#5016);
#4277=LINE('',#21611,#5017);
#4278=LINE('',#21620,#5018);
#4279=LINE('',#21626,#5019);
#4280=LINE('',#21635,#5020);
#4281=LINE('',#21641,#5021);
#4282=LINE('',#21649,#5022);
#4283=LINE('',#21651,#5023);
#4284=LINE('',#21653,#5024);
#4285=LINE('',#21654,#5025);
#4286=LINE('',#21657,#5026);
#4287=LINE('',#21659,#5027);
#4288=LINE('',#21660,#5028);
#4289=LINE('',#21663,#5029);
#4290=LINE('',#21665,#5030);
#4291=LINE('',#21666,#5031);
#4292=LINE('',#21669,#5032);
#4293=LINE('',#21671,#5033);
#4294=LINE('',#21672,#5034);
#4295=LINE('',#21675,#5035);
#4296=LINE('',#21677,#5036);
#4297=LINE('',#21678,#5037);
#4298=LINE('',#21680,#5038);
#4299=LINE('',#21681,#5039);
#4300=LINE('',#21693,#5040);
#4301=LINE('',#21697,#5041);
#4302=LINE('',#21701,#5042);
#4303=LINE('',#21708,#5043);
#4304=LINE('',#21710,#5044);
#4305=LINE('',#21717,#5045);
#4306=LINE('',#21723,#5046);
#4307=LINE('',#21729,#5047);
#4308=LINE('',#21735,#5048);
#4309=LINE('',#21741,#5049);
#4310=LINE('',#21747,#5050);
#4311=LINE('',#21753,#5051);
#4312=LINE('',#21759,#5052);
#4313=LINE('',#21764,#5053);
#4314=LINE('',#21766,#5054);
#4315=LINE('',#21768,#5055);
#4316=LINE('',#21769,#5056);
#4317=LINE('',#21772,#5057);
#4318=LINE('',#21774,#5058);
#4319=LINE('',#21775,#5059);
#4320=LINE('',#21778,#5060);
#4321=LINE('',#21780,#5061);
#4322=LINE('',#21781,#5062);
#4323=LINE('',#21783,#5063);
#4324=LINE('',#21784,#5064);
#4325=LINE('',#21792,#5065);
#4326=LINE('',#21798,#5066);
#4327=LINE('',#21804,#5067);
#4328=LINE('',#21810,#5068);
#4329=LINE('',#21815,#5069);
#4330=LINE('',#21817,#5070);
#4331=LINE('',#21819,#5071);
#4332=LINE('',#21820,#5072);
#4333=LINE('',#21823,#5073);
#4334=LINE('',#21825,#5074);
#4335=LINE('',#21827,#5075);
#4336=LINE('',#21828,#5076);
#4337=LINE('',#21831,#5077);
#4338=LINE('',#21833,#5078);
#4339=LINE('',#21834,#5079);
#4340=LINE('',#21837,#5080);
#4341=LINE('',#21838,#5081);
#4342=LINE('',#21841,#5082);
#4343=LINE('',#21842,#5083);
#4344=LINE('',#21844,#5084);
#4345=LINE('',#21847,#5085);
#4346=LINE('',#21849,#5086);
#4347=LINE('',#21850,#5087);
#4348=LINE('',#21855,#5088);
#4349=LINE('',#21856,#5089);
#4350=LINE('',#21863,#5090);
#4351=LINE('',#21867,#5091);
#4352=LINE('',#21871,#5092);
#4353=LINE('',#21875,#5093);
#4354=LINE('',#21876,#5094);
#4355=LINE('',#21878,#5095);
#4356=LINE('',#21886,#5096);
#4357=LINE('',#21892,#5097);
#4358=LINE('',#21898,#5098);
#4359=LINE('',#21904,#5099);
#4360=LINE('',#21909,#5100);
#4361=LINE('',#21911,#5101);
#4362=LINE('',#21913,#5102);
#4363=LINE('',#21914,#5103);
#4364=LINE('',#21918,#5104);
#4365=LINE('',#21920,#5105);
#4366=LINE('',#21922,#5106);
#4367=LINE('',#21923,#5107);
#4368=LINE('',#21926,#5108);
#4369=LINE('',#21928,#5109);
#4370=LINE('',#21929,#5110);
#4371=LINE('',#21933,#5111);
#4372=LINE('',#21934,#5112);
#4373=LINE('',#21935,#5113);
#4374=LINE('',#21938,#5114);
#4375=LINE('',#21940,#5115);
#4376=LINE('',#21941,#5116);
#4377=LINE('',#21948,#5117);
#4378=LINE('',#21949,#5118);
#4379=LINE('',#21950,#5119);
#4380=LINE('',#21954,#5120);
#4381=LINE('',#21958,#5121);
#4382=LINE('',#21961,#5122);
#4383=LINE('',#21962,#5123);
#4384=LINE('',#21963,#5124);
#4385=LINE('',#21965,#5125);
#4386=LINE('',#21973,#5126);
#4387=LINE('',#21982,#5127);
#4388=LINE('',#21991,#5128);
#4389=LINE('',#21998,#5129);
#4390=LINE('',#22005,#5130);
#4391=LINE('',#22014,#5131);
#4392=LINE('',#22020,#5132);
#4393=LINE('',#22029,#5133);
#4394=LINE('',#22035,#5134);
#4395=LINE('',#22044,#5135);
#4396=LINE('',#22050,#5136);
#4397=LINE('',#22059,#5137);
#4398=LINE('',#22065,#5138);
#4399=LINE('',#22074,#5139);
#4400=LINE('',#22080,#5140);
#4401=LINE('',#22089,#5141);
#4402=LINE('',#22095,#5142);
#4403=LINE('',#22106,#5143);
#4404=LINE('',#22110,#5144);
#4405=LINE('',#22114,#5145);
#4406=LINE('',#22121,#5146);
#4407=LINE('',#22125,#5147);
#4408=LINE('',#22129,#5148);
#4409=LINE('',#22134,#5149);
#4410=LINE('',#22136,#5150);
#4411=LINE('',#22138,#5151);
#4412=LINE('',#22139,#5152);
#4413=LINE('',#22142,#5153);
#4414=LINE('',#22144,#5154);
#4415=LINE('',#22145,#5155);
#4416=LINE('',#22148,#5156);
#4417=LINE('',#22150,#5157);
#4418=LINE('',#22151,#5158);
#4419=LINE('',#22154,#5159);
#4420=LINE('',#22156,#5160);
#4421=LINE('',#22157,#5161);
#4422=LINE('',#22160,#5162);
#4423=LINE('',#22162,#5163);
#4424=LINE('',#22163,#5164);
#4425=LINE('',#22165,#5165);
#4426=LINE('',#22166,#5166);
#4427=LINE('',#22175,#5167);
#4428=LINE('',#22181,#5168);
#4429=LINE('',#22187,#5169);
#4430=LINE('',#22192,#5170);
#4431=LINE('',#22194,#5171);
#4432=LINE('',#22196,#5172);
#4433=LINE('',#22197,#5173);
#4434=LINE('',#22200,#5174);
#4435=LINE('',#22202,#5175);
#4436=LINE('',#22203,#5176);
#4437=LINE('',#22206,#5177);
#4438=LINE('',#22208,#5178);
#4439=LINE('',#22209,#5179);
#4440=LINE('',#22211,#5180);
#4441=LINE('',#22212,#5181);
#4442=LINE('',#22220,#5182);
#4443=LINE('',#22229,#5183);
#4444=LINE('',#22238,#5184);
#4445=LINE('',#22243,#5185);
#4446=LINE('',#22247,#5186);
#4447=LINE('',#22251,#5187);
#4448=LINE('',#22253,#5188);
#4449=LINE('',#22255,#5189);
#4450=LINE('',#22256,#5190);
#4451=LINE('',#22259,#5191);
#4452=LINE('',#22261,#5192);
#4453=LINE('',#22262,#5193);
#4454=LINE('',#22265,#5194);
#4455=LINE('',#22267,#5195);
#4456=LINE('',#22268,#5196);
#4457=LINE('',#22270,#5197);
#4458=LINE('',#22271,#5198);
#4459=LINE('',#22279,#5199);
#4460=LINE('',#22288,#5200);
#4461=LINE('',#22297,#5201);
#4462=LINE('',#22301,#5202);
#4463=LINE('',#22305,#5203);
#4464=LINE('',#22310,#5204);
#4465=LINE('',#22312,#5205);
#4466=LINE('',#22314,#5206);
#4467=LINE('',#22315,#5207);
#4468=LINE('',#22318,#5208);
#4469=LINE('',#22320,#5209);
#4470=LINE('',#22321,#5210);
#4471=LINE('',#22324,#5211);
#4472=LINE('',#22326,#5212);
#4473=LINE('',#22327,#5213);
#4474=LINE('',#22329,#5214);
#4475=LINE('',#22330,#5215);
#4476=LINE('',#22337,#5216);
#4477=LINE('',#22358,#5217);
#4478=LINE('',#22377,#5218);
#4479=LINE('',#22382,#5219);
#4480=LINE('',#22387,#5220);
#4481=LINE('',#22389,#5221);
#4482=LINE('',#22391,#5222);
#4483=LINE('',#22392,#5223);
#4484=LINE('',#22395,#5224);
#4485=LINE('',#22397,#5225);
#4486=LINE('',#22398,#5226);
#4487=LINE('',#22401,#5227);
#4488=LINE('',#22403,#5228);
#4489=LINE('',#22404,#5229);
#4490=LINE('',#22406,#5230);
#4491=LINE('',#22407,#5231);
#4492=LINE('',#22415,#5232);
#4493=LINE('',#22422,#5233);
#4494=LINE('',#22429,#5234);
#4495=LINE('',#22438,#5235);
#4496=LINE('',#22444,#5236);
#4497=LINE('',#22453,#5237);
#4498=LINE('',#22459,#5238);
#4499=LINE('',#22468,#5239);
#4500=LINE('',#22474,#5240);
#4501=LINE('',#22483,#5241);
#4502=LINE('',#22489,#5242);
#4503=LINE('',#22498,#5243);
#4504=LINE('',#22504,#5244);
#4505=LINE('',#22513,#5245);
#4506=LINE('',#22519,#5246);
#4507=LINE('',#22529,#5247);
#4508=LINE('',#22535,#5248);
#4509=LINE('',#22541,#5249);
#4510=LINE('',#22546,#5250);
#4511=LINE('',#22548,#5251);
#4512=LINE('',#22550,#5252);
#4513=LINE('',#22551,#5253);
#4514=LINE('',#22554,#5254);
#4515=LINE('',#22556,#5255);
#4516=LINE('',#22557,#5256);
#4517=LINE('',#22560,#5257);
#4518=LINE('',#22562,#5258);
#4519=LINE('',#22563,#5259);
#4520=LINE('',#22565,#5260);
#4521=LINE('',#22566,#5261);
#4522=LINE('',#22574,#5262);
#4523=LINE('',#22583,#5263);
#4524=LINE('',#22592,#5264);
#4525=LINE('',#22597,#5265);
#4526=LINE('',#22601,#5266);
#4527=LINE('',#22605,#5267);
#4528=LINE('',#22607,#5268);
#4529=LINE('',#22609,#5269);
#4530=LINE('',#22610,#5270);
#4531=LINE('',#22613,#5271);
#4532=LINE('',#22615,#5272);
#4533=LINE('',#22616,#5273);
#4534=LINE('',#22619,#5274);
#4535=LINE('',#22621,#5275);
#4536=LINE('',#22622,#5276);
#4537=LINE('',#22624,#5277);
#4538=LINE('',#22625,#5278);
#4539=LINE('',#22633,#5279);
#4540=LINE('',#22642,#5280);
#4541=LINE('',#22651,#5281);
#4542=LINE('',#22655,#5282);
#4543=LINE('',#22659,#5283);
#4544=LINE('',#22664,#5284);
#4545=LINE('',#22666,#5285);
#4546=LINE('',#22668,#5286);
#4547=LINE('',#22669,#5287);
#4548=LINE('',#22672,#5288);
#4549=LINE('',#22674,#5289);
#4550=LINE('',#22675,#5290);
#4551=LINE('',#22678,#5291);
#4552=LINE('',#22680,#5292);
#4553=LINE('',#22681,#5293);
#4554=LINE('',#22683,#5294);
#4555=LINE('',#22684,#5295);
#4556=LINE('',#22691,#5296);
#4557=LINE('',#22712,#5297);
#4558=LINE('',#22731,#5298);
#4559=LINE('',#22736,#5299);
#4560=LINE('',#22741,#5300);
#4561=LINE('',#22743,#5301);
#4562=LINE('',#22745,#5302);
#4563=LINE('',#22746,#5303);
#4564=LINE('',#22749,#5304);
#4565=LINE('',#22751,#5305);
#4566=LINE('',#22752,#5306);
#4567=LINE('',#22755,#5307);
#4568=LINE('',#22757,#5308);
#4569=LINE('',#22758,#5309);
#4570=LINE('',#22760,#5310);
#4571=LINE('',#22761,#5311);
#4572=LINE('',#22769,#5312);
#4573=LINE('',#22776,#5313);
#4574=LINE('',#22783,#5314);
#4575=LINE('',#22792,#5315);
#4576=LINE('',#22798,#5316);
#4577=LINE('',#22807,#5317);
#4578=LINE('',#22813,#5318);
#4579=LINE('',#22822,#5319);
#4580=LINE('',#22828,#5320);
#4581=LINE('',#22837,#5321);
#4582=LINE('',#22843,#5322);
#4583=LINE('',#22852,#5323);
#4584=LINE('',#22858,#5324);
#4585=LINE('',#22867,#5325);
#4586=LINE('',#22873,#5326);
#4587=LINE('',#22884,#5327);
#4588=LINE('',#22886,#5328);
#4589=LINE('',#22887,#5329);
#4590=LINE('',#22890,#5330);
#4591=LINE('',#22892,#5331);
#4592=LINE('',#22893,#5332);
#4593=LINE('',#22898,#5333);
#4594=LINE('',#22899,#5334);
#4595=LINE('',#22901,#5335);
#4596=LINE('',#22902,#5336);
#4597=LINE('',#22912,#5337);
#4598=LINE('',#22919,#5338);
#4599=LINE('',#22926,#5339);
#4600=LINE('',#22933,#5340);
#4601=LINE('',#22940,#5341);
#4602=LINE('',#22945,#5342);
#4603=LINE('',#22952,#5343);
#4604=LINE('',#22955,#5344);
#4605=LINE('',#22958,#5345);
#4606=LINE('',#22960,#5346);
#4607=LINE('',#22961,#5347);
#4608=LINE('',#22967,#5348);
#4609=LINE('',#22969,#5349);
#4610=LINE('',#22970,#5350);
#4611=LINE('',#22979,#5351);
#4612=LINE('',#22984,#5352);
#4613=LINE('',#22994,#5353);
#4614=LINE('',#22996,#5354);
#4615=LINE('',#22998,#5355);
#4616=LINE('',#22999,#5356);
#4617=LINE('',#23002,#5357);
#4618=LINE('',#23004,#5358);
#4619=LINE('',#23005,#5359);
#4620=LINE('',#23008,#5360);
#4621=LINE('',#23010,#5361);
#4622=LINE('',#23011,#5362);
#4623=LINE('',#23014,#5363);
#4624=LINE('',#23016,#5364);
#4625=LINE('',#23017,#5365);
#4626=LINE('',#23020,#5366);
#4627=LINE('',#23022,#5367);
#4628=LINE('',#23023,#5368);
#4629=LINE('',#23025,#5369);
#4630=LINE('',#23026,#5370);
#4631=LINE('',#23034,#5371);
#4632=LINE('',#23036,#5372);
#4633=LINE('',#23043,#5373);
#4634=LINE('',#23048,#5374);
#4635=LINE('',#23052,#5375);
#4636=LINE('',#23057,#5376);
#4637=LINE('',#23061,#5377);
#4638=LINE('',#23065,#5378);
#4639=LINE('',#23067,#5379);
#4640=LINE('',#23068,#5380);
#4641=LINE('',#23071,#5381);
#4642=LINE('',#23073,#5382);
#4643=LINE('',#23074,#5383);
#4644=LINE('',#23077,#5384);
#4645=LINE('',#23079,#5385);
#4646=LINE('',#23080,#5386);
#4647=LINE('',#23085,#5387);
#4648=LINE('',#23092,#5388);
#4649=LINE('',#23098,#5389);
#4650=LINE('',#23099,#5390);
#4651=LINE('',#23102,#5391);
#4652=LINE('',#23112,#5392);
#4653=LINE('',#23118,#5393);
#4654=LINE('',#23127,#5394);
#4655=LINE('',#23133,#5395);
#4656=LINE('',#23142,#5396);
#4657=LINE('',#23148,#5397);
#4658=LINE('',#23157,#5398);
#4659=LINE('',#23162,#5399);
#4660=LINE('',#23166,#5400);
#4661=LINE('',#23171,#5401);
#4662=LINE('',#23175,#5402);
#4663=LINE('',#23179,#5403);
#4664=LINE('',#23181,#5404);
#4665=LINE('',#23182,#5405);
#4666=LINE('',#23185,#5406);
#4667=LINE('',#23187,#5407);
#4668=LINE('',#23188,#5408);
#4669=LINE('',#23191,#5409);
#4670=LINE('',#23193,#5410);
#4671=LINE('',#23194,#5411);
#4672=LINE('',#23199,#5412);
#4673=LINE('',#23206,#5413);
#4674=LINE('',#23212,#5414);
#4675=LINE('',#23213,#5415);
#4676=LINE('',#23216,#5416);
#4677=LINE('',#23226,#5417);
#4678=LINE('',#23232,#5418);
#4679=LINE('',#23241,#5419);
#4680=LINE('',#23247,#5420);
#4681=LINE('',#23256,#5421);
#4682=LINE('',#23262,#5422);
#4683=LINE('',#23271,#5423);
#4684=LINE('',#23278,#5424);
#4685=LINE('',#23285,#5425);
#4686=LINE('',#23294,#5426);
#4687=LINE('',#23300,#5427);
#4688=LINE('',#23309,#5428);
#4689=LINE('',#23315,#5429);
#4690=LINE('',#23324,#5430);
#4691=LINE('',#23330,#5431);
#4692=LINE('',#23339,#5432);
#4693=LINE('',#23345,#5433);
#4694=LINE('',#23354,#5434);
#4695=LINE('',#23360,#5435);
#4696=LINE('',#23369,#5436);
#4697=LINE('',#23375,#5437);
#4698=LINE('',#23384,#5438);
#4699=LINE('',#23390,#5439);
#4700=LINE('',#23401,#5440);
#4701=LINE('',#23405,#5441);
#4702=LINE('',#23409,#5442);
#4703=LINE('',#23416,#5443);
#4704=LINE('',#23420,#5444);
#4705=LINE('',#23424,#5445);
#4706=LINE('',#23429,#5446);
#4707=LINE('',#23431,#5447);
#4708=LINE('',#23433,#5448);
#4709=LINE('',#23434,#5449);
#4710=LINE('',#23437,#5450);
#4711=LINE('',#23439,#5451);
#4712=LINE('',#23440,#5452);
#4713=LINE('',#23443,#5453);
#4714=LINE('',#23445,#5454);
#4715=LINE('',#23446,#5455);
#4716=LINE('',#23449,#5456);
#4717=LINE('',#23451,#5457);
#4718=LINE('',#23452,#5458);
#4719=LINE('',#23455,#5459);
#4720=LINE('',#23457,#5460);
#4721=LINE('',#23458,#5461);
#4722=LINE('',#23460,#5462);
#4723=LINE('',#23461,#5463);
#4724=LINE('',#23542,#5464);
#4725=LINE('',#23548,#5465);
#4726=LINE('',#23554,#5466);
#4727=LINE('',#23560,#5467);
#4728=LINE('',#23566,#5468);
#4729=LINE('',#23571,#5469);
#4730=LINE('',#23575,#5470);
#4731=LINE('',#23580,#5471);
#4732=LINE('',#23584,#5472);
#4733=LINE('',#23588,#5473);
#4734=LINE('',#23590,#5474);
#4735=LINE('',#23591,#5475);
#4736=LINE('',#23595,#5476);
#4737=LINE('',#23597,#5477);
#4738=LINE('',#23600,#5478);
#4739=LINE('',#23607,#5479);
#4740=LINE('',#23608,#5480);
#4741=LINE('',#23612,#5481);
#4742=LINE('',#23615,#5482);
#4743=LINE('',#23618,#5483);
#4744=LINE('',#23620,#5484);
#4745=LINE('',#23624,#5485);
#4746=LINE('',#23628,#5486);
#4747=LINE('',#23635,#5487);
#4748=LINE('',#23641,#5488);
#4749=LINE('',#23650,#5489);
#4750=LINE('',#23656,#5490);
#4751=LINE('',#23665,#5491);
#4752=LINE('',#23671,#5492);
#4753=LINE('',#23677,#5493);
#4754=LINE('',#23683,#5494);
#4755=LINE('',#23689,#5495);
#4756=LINE('',#23695,#5496);
#4757=LINE('',#23707,#5497);
#4758=LINE('',#23713,#5498);
#4759=LINE('',#23723,#5499);
#4760=LINE('',#23729,#5500);
#4761=LINE('',#23739,#5501);
#4762=LINE('',#23745,#5502);
#4763=LINE('',#23755,#5503);
#4764=LINE('',#23761,#5504);
#4765=LINE('',#23768,#5505);
#4766=LINE('',#23774,#5506);
#4767=LINE('',#23780,#5507);
#4768=LINE('',#23786,#5508);
#4769=LINE('',#23792,#5509);
#4770=LINE('',#23798,#5510);
#4771=LINE('',#23811,#5511);
#4772=LINE('',#23815,#5512);
#4773=LINE('',#23827,#5513);
#4774=LINE('',#23831,#5514);
#4775=LINE('',#23843,#5515);
#4776=LINE('',#23847,#5516);
#4777=LINE('',#23859,#5517);
#4778=LINE('',#23863,#5518);
#4779=LINE('',#23871,#5519);
#4780=LINE('',#23877,#5520);
#4781=LINE('',#23883,#5521);
#4782=LINE('',#23889,#5522);
#4783=LINE('',#23895,#5523);
#4784=LINE('',#23900,#5524);
#4785=LINE('',#23904,#5525);
#4786=LINE('',#23909,#5526);
#4787=LINE('',#23913,#5527);
#4788=LINE('',#23917,#5528);
#4789=LINE('',#23919,#5529);
#4790=LINE('',#23920,#5530);
#4791=LINE('',#23924,#5531);
#4792=LINE('',#23926,#5532);
#4793=LINE('',#23929,#5533);
#4794=LINE('',#23936,#5534);
#4795=LINE('',#23937,#5535);
#4796=LINE('',#23941,#5536);
#4797=LINE('',#23944,#5537);
#4798=LINE('',#23947,#5538);
#4799=LINE('',#23949,#5539);
#4800=LINE('',#23953,#5540);
#4801=LINE('',#23957,#5541);
#4802=LINE('',#23964,#5542);
#4803=LINE('',#23970,#5543);
#4804=LINE('',#23979,#5544);
#4805=LINE('',#23985,#5545);
#4806=LINE('',#23994,#5546);
#4807=LINE('',#24000,#5547);
#4808=LINE('',#24006,#5548);
#4809=LINE('',#24012,#5549);
#4810=LINE('',#24018,#5550);
#4811=LINE('',#24024,#5551);
#4812=LINE('',#24036,#5552);
#4813=LINE('',#24042,#5553);
#4814=LINE('',#24052,#5554);
#4815=LINE('',#24058,#5555);
#4816=LINE('',#24068,#5556);
#4817=LINE('',#24074,#5557);
#4818=LINE('',#24084,#5558);
#4819=LINE('',#24090,#5559);
#4820=LINE('',#24097,#5560);
#4821=LINE('',#24103,#5561);
#4822=LINE('',#24109,#5562);
#4823=LINE('',#24115,#5563);
#4824=LINE('',#24121,#5564);
#4825=LINE('',#24127,#5565);
#4826=LINE('',#24140,#5566);
#4827=LINE('',#24144,#5567);
#4828=LINE('',#24156,#5568);
#4829=LINE('',#24160,#5569);
#4830=LINE('',#24172,#5570);
#4831=LINE('',#24176,#5571);
#4832=LINE('',#24188,#5572);
#4833=LINE('',#24192,#5573);
#4834=LINE('',#24209,#5574);
#4835=LINE('',#24215,#5575);
#4836=LINE('',#24219,#5576);
#4837=LINE('',#24225,#5577);
#4838=LINE('',#24230,#5578);
#4839=LINE('',#24245,#5579);
#4840=LINE('',#24254,#5580);
#4841=LINE('',#24258,#5581);
#4842=LINE('',#24262,#5582);
#4843=LINE('',#24265,#5583);
#4844=LINE('',#24627,#5584);
#4845=LINE('',#24632,#5585);
#4846=LINE('',#24641,#5586);
#4847=LINE('',#24646,#5587);
#4848=LINE('',#24738,#5588);
#4849=LINE('',#24741,#5589);
#4850=LINE('',#24752,#5590);
#4851=LINE('',#24755,#5591);
#4852=LINE('',#24760,#5592);
#4853=LINE('',#24768,#5593);
#4854=LINE('',#24774,#5594);
#4855=LINE('',#24783,#5595);
#4856=LINE('',#24789,#5596);
#4857=LINE('',#24798,#5597);
#4858=LINE('',#24804,#5598);
#4859=LINE('',#24813,#5599);
#4860=LINE('',#24819,#5600);
#4861=LINE('',#24828,#5601);
#4862=LINE('',#24835,#5602);
#4863=LINE('',#24841,#5603);
#4864=VECTOR('',#16478,0.210000000000001);
#4865=VECTOR('',#16485,0.210000000000001);
#4866=VECTOR('',#16492,0.210000000000001);
#4867=VECTOR('',#16499,0.210000000000001);
#4868=VECTOR('',#16506,0.21);
#4869=VECTOR('',#16513,0.21);
#4870=VECTOR('',#16520,0.21);
#4871=VECTOR('',#16527,0.21);
#4872=VECTOR('',#16532,1.);
#4873=VECTOR('',#16533,1.);
#4874=VECTOR('',#16534,1.);
#4875=VECTOR('',#16535,1.);
#4876=VECTOR('',#16538,1.);
#4877=VECTOR('',#16539,1.);
#4878=VECTOR('',#16540,1.);
#4879=VECTOR('',#16543,1.);
#4880=VECTOR('',#16544,1.);
#4881=VECTOR('',#16545,1.);
#4882=VECTOR('',#16548,1.);
#4883=VECTOR('',#16549,1.);
#4884=VECTOR('',#16558,1.);
#4885=VECTOR('',#16559,1.);
#4886=VECTOR('',#16560,1.);
#4887=VECTOR('',#16561,1.);
#4888=VECTOR('',#16564,1.);
#4889=VECTOR('',#16565,1.);
#4890=VECTOR('',#16566,1.);
#4891=VECTOR('',#16569,1.);
#4892=VECTOR('',#16570,1.);
#4893=VECTOR('',#16571,1.);
#4894=VECTOR('',#16574,1.);
#4895=VECTOR('',#16575,1.);
#4896=VECTOR('',#16584,1.);
#4897=VECTOR('',#16585,1.);
#4898=VECTOR('',#16586,1.);
#4899=VECTOR('',#16587,1.);
#4900=VECTOR('',#16590,1.);
#4901=VECTOR('',#16591,1.);
#4902=VECTOR('',#16592,1.);
#4903=VECTOR('',#16595,1.);
#4904=VECTOR('',#16596,1.);
#4905=VECTOR('',#16597,1.);
#4906=VECTOR('',#16600,1.);
#4907=VECTOR('',#16601,1.);
#4908=VECTOR('',#16612,0.165);
#4909=VECTOR('',#16619,0.165);
#4910=VECTOR('',#16626,0.165);
#4911=VECTOR('',#16633,0.165);
#4912=VECTOR('',#16640,1.6);
#4913=VECTOR('',#16647,0.275);
#4914=VECTOR('',#16654,0.275);
#4915=VECTOR('',#16661,0.275);
#4916=VECTOR('',#16668,0.275);
#4917=VECTOR('',#16673,1.);
#4918=VECTOR('',#16674,1.);
#4919=VECTOR('',#16675,1.);
#4920=VECTOR('',#16676,1.);
#4921=VECTOR('',#16679,1.);
#4922=VECTOR('',#16680,1.);
#4923=VECTOR('',#16681,1.);
#4924=VECTOR('',#16682,1.);
#4925=VECTOR('',#16685,1.);
#4926=VECTOR('',#16686,1.);
#4927=VECTOR('',#16687,1.);
#4928=VECTOR('',#16690,1.);
#4929=VECTOR('',#16691,1.);
#4930=VECTOR('',#16692,1.);
#4931=VECTOR('',#16695,1.);
#4932=VECTOR('',#16696,1.);
#4933=VECTOR('',#16697,1.);
#4934=VECTOR('',#16698,1.);
#4935=VECTOR('',#16703,1.);
#4936=VECTOR('',#16704,1.);
#4937=VECTOR('',#16713,0.605);
#4938=VECTOR('',#16716,0.605);
#4939=VECTOR('',#16721,0.605);
#4940=VECTOR('',#16726,1.);
#4941=VECTOR('',#16727,1.);
#4942=VECTOR('',#16730,1.);
#4943=VECTOR('',#16731,1.);
#4944=VECTOR('',#16742,0.225);
#4945=VECTOR('',#16749,0.225);
#4946=VECTOR('',#16756,0.225);
#4947=VECTOR('',#16763,0.225);
#4948=VECTOR('',#16770,1.59);
#4949=VECTOR('',#16779,1.02);
#4950=VECTOR('',#16786,2.2);
#4951=VECTOR('',#16799,0.225);
#4952=VECTOR('',#16806,0.225);
#4953=VECTOR('',#16813,0.225);
#4954=VECTOR('',#16820,0.225);
#4955=VECTOR('',#16827,1.59);
#4956=VECTOR('',#16838,1.02);
#4957=VECTOR('',#16843,2.2);
#4958=VECTOR('',#16856,0.165);
#4959=VECTOR('',#16863,0.165);
#4960=VECTOR('',#16870,0.165);
#4961=VECTOR('',#16877,0.165);
#4962=VECTOR('',#16884,1.6);
#4963=VECTOR('',#16891,0.274999999999999);
#4964=VECTOR('',#16898,0.274999999999999);
#4965=VECTOR('',#16905,0.274999999999999);
#4966=VECTOR('',#16912,0.274999999999999);
#4967=VECTOR('',#16917,1.);
#4968=VECTOR('',#16918,1.);
#4969=VECTOR('',#16919,1.);
#4970=VECTOR('',#16920,1.);
#4971=VECTOR('',#16923,1.);
#4972=VECTOR('',#16924,1.);
#4973=VECTOR('',#16925,1.);
#4974=VECTOR('',#16926,1.);
#4975=VECTOR('',#16929,1.);
#4976=VECTOR('',#16930,1.);
#4977=VECTOR('',#16931,1.);
#4978=VECTOR('',#16934,1.);
#4979=VECTOR('',#16935,1.);
#4980=VECTOR('',#16936,1.);
#4981=VECTOR('',#16939,1.);
#4982=VECTOR('',#16940,1.);
#4983=VECTOR('',#16941,1.);
#4984=VECTOR('',#16942,1.);
#4985=VECTOR('',#16945,1.);
#4986=VECTOR('',#16946,1.);
#4987=VECTOR('',#16953,0.605);
#4988=VECTOR('',#16958,0.605);
#4989=VECTOR('',#16963,1.);
#4990=VECTOR('',#16964,1.);
#4991=VECTOR('',#16967,1.);
#4992=VECTOR('',#16968,1.);
#4993=VECTOR('',#16979,0.225);
#4994=VECTOR('',#16986,0.225);
#4995=VECTOR('',#16993,0.225);
#4996=VECTOR('',#17000,0.225);
#4997=VECTOR('',#17007,1.59);
#4998=VECTOR('',#17016,1.02);
#4999=VECTOR('',#17023,2.2);
#5000=VECTOR('',#17036,0.225);
#5001=VECTOR('',#17043,0.225);
#5002=VECTOR('',#17050,0.225);
#5003=VECTOR('',#17057,0.225);
#5004=VECTOR('',#17064,1.59);
#5005=VECTOR('',#17075,1.02);
#5006=VECTOR('',#17080,2.2);
#5007=VECTOR('',#17093,0.6);
#5008=VECTOR('',#17106,0.6);
#5009=VECTOR('',#17119,0.165);
#5010=VECTOR('',#17128,0.165);
#5011=VECTOR('',#17137,0.6);
#5012=VECTOR('',#17150,0.225);
#5013=VECTOR('',#17157,1.);
#5014=VECTOR('',#17170,0.225);
#5015=VECTOR('',#17177,1.);
#5016=VECTOR('',#17190,0.605);
#5017=VECTOR('',#17197,0.8);
#5018=VECTOR('',#17210,0.605);
#5019=VECTOR('',#17217,0.8);
#5020=VECTOR('',#17230,0.605);
#5021=VECTOR('',#17237,0.8);
#5022=VECTOR('',#17248,1.);
#5023=VECTOR('',#17249,1.);
#5024=VECTOR('',#17250,1.);
#5025=VECTOR('',#17251,1.);
#5026=VECTOR('',#17254,1.);
#5027=VECTOR('',#17255,1.);
#5028=VECTOR('',#17256,1.);
#5029=VECTOR('',#17259,1.);
#5030=VECTOR('',#17260,1.);
#5031=VECTOR('',#17261,1.);
#5032=VECTOR('',#17264,1.);
#5033=VECTOR('',#17265,1.);
#5034=VECTOR('',#17266,1.);
#5035=VECTOR('',#17269,1.);
#5036=VECTOR('',#17270,1.);
#5037=VECTOR('',#17271,1.);
#5038=VECTOR('',#17274,1.);
#5039=VECTOR('',#17275,1.);
#5040=VECTOR('',#17292,0.325);
#5041=VECTOR('',#17297,0.35);
#5042=VECTOR('',#17302,0.335);
#5043=VECTOR('',#17311,0.21);
#5044=VECTOR('',#17314,0.2);
#5045=VECTOR('',#17323,0.274999999999999);
#5046=VECTOR('',#17330,0.274999999999999);
#5047=VECTOR('',#17337,0.274999999999999);
#5048=VECTOR('',#17344,0.274999999999999);
#5049=VECTOR('',#17351,0.275);
#5050=VECTOR('',#17358,0.275);
#5051=VECTOR('',#17365,0.275);
#5052=VECTOR('',#17372,0.275);
#5053=VECTOR('',#17377,1.);
#5054=VECTOR('',#17378,1.);
#5055=VECTOR('',#17379,1.);
#5056=VECTOR('',#17380,1.);
#5057=VECTOR('',#17383,1.);
#5058=VECTOR('',#17384,1.);
#5059=VECTOR('',#17385,1.);
#5060=VECTOR('',#17388,1.);
#5061=VECTOR('',#17389,1.);
#5062=VECTOR('',#17390,1.);
#5063=VECTOR('',#17393,1.);
#5064=VECTOR('',#17394,1.);
#5065=VECTOR('',#17405,0.21);
#5066=VECTOR('',#17412,0.21);
#5067=VECTOR('',#17419,0.21);
#5068=VECTOR('',#17426,0.21);
#5069=VECTOR('',#17431,1.);
#5070=VECTOR('',#17432,1.);
#5071=VECTOR('',#17433,1.);
#5072=VECTOR('',#17434,1.);
#5073=VECTOR('',#17435,1.);
#5074=VECTOR('',#17436,1.);
#5075=VECTOR('',#17437,1.);
#5076=VECTOR('',#17438,1.);
#5077=VECTOR('',#17441,1.);
#5078=VECTOR('',#17442,1.);
#5079=VECTOR('',#17443,1.);
#5080=VECTOR('',#17446,1.);
#5081=VECTOR('',#17447,1.);
#5082=VECTOR('',#17450,1.);
#5083=VECTOR('',#17451,1.);
#5084=VECTOR('',#17454,1.);
#5085=VECTOR('',#17457,1.);
#5086=VECTOR('',#17458,1.);
#5087=VECTOR('',#17459,1.);
#5088=VECTOR('',#17464,1.);
#5089=VECTOR('',#17465,1.);
#5090=VECTOR('',#17472,0.605);
#5091=VECTOR('',#17477,0.605);
#5092=VECTOR('',#17482,0.605);
#5093=VECTOR('',#17487,1.);
#5094=VECTOR('',#17488,1.);
#5095=VECTOR('',#17491,1.);
#5096=VECTOR('',#17502,0.210000000000001);
#5097=VECTOR('',#17509,0.210000000000001);
#5098=VECTOR('',#17516,0.210000000000001);
#5099=VECTOR('',#17523,0.210000000000001);
#5100=VECTOR('',#17528,1.);
#5101=VECTOR('',#17529,1.);
#5102=VECTOR('',#17530,1.);
#5103=VECTOR('',#17531,1.);
#5104=VECTOR('',#17534,1.);
#5105=VECTOR('',#17535,1.);
#5106=VECTOR('',#17536,1.);
#5107=VECTOR('',#17537,1.);
#5108=VECTOR('',#17540,1.);
#5109=VECTOR('',#17541,1.);
#5110=VECTOR('',#17542,1.);
#5111=VECTOR('',#17545,1.);
#5112=VECTOR('',#17546,1.);
#5113=VECTOR('',#17547,1.);
#5114=VECTOR('',#17550,1.);
#5115=VECTOR('',#17551,1.);
#5116=VECTOR('',#17552,1.);
#5117=VECTOR('',#17559,1.);
#5118=VECTOR('',#17560,1.);
#5119=VECTOR('',#17561,1.);
#5120=VECTOR('',#17566,0.605);
#5121=VECTOR('',#17571,0.605);
#5122=VECTOR('',#17574,1.);
#5123=VECTOR('',#17575,1.);
#5124=VECTOR('',#17576,1.);
#5125=VECTOR('',#17579,1.);
#5126=VECTOR('',#17590,0.6);
#5127=VECTOR('',#17603,0.6);
#5128=VECTOR('',#17616,0.165);
#5129=VECTOR('',#17625,0.165);
#5130=VECTOR('',#17634,0.6);
#5131=VECTOR('',#17647,0.225);
#5132=VECTOR('',#17654,1.);
#5133=VECTOR('',#17667,0.225);
#5134=VECTOR('',#17674,1.);
#5135=VECTOR('',#17687,0.605);
#5136=VECTOR('',#17694,0.8);
#5137=VECTOR('',#17707,0.605);
#5138=VECTOR('',#17714,0.8);
#5139=VECTOR('',#17727,0.605);
#5140=VECTOR('',#17734,0.8);
#5141=VECTOR('',#17747,0.605);
#5142=VECTOR('',#17754,0.8);
#5143=VECTOR('',#17771,0.4);
#5144=VECTOR('',#17776,0.425);
#5145=VECTOR('',#17781,0.41);
#5146=VECTOR('',#17790,0.26);
#5147=VECTOR('',#17795,0.25);
#5148=VECTOR('',#17800,0.225);
#5149=VECTOR('',#17805,1.);
#5150=VECTOR('',#17806,1.);
#5151=VECTOR('',#17807,1.);
#5152=VECTOR('',#17808,1.);
#5153=VECTOR('',#17811,1.);
#5154=VECTOR('',#17812,1.);
#5155=VECTOR('',#17813,1.);
#5156=VECTOR('',#17816,1.);
#5157=VECTOR('',#17817,1.);
#5158=VECTOR('',#17818,1.);
#5159=VECTOR('',#17821,1.);
#5160=VECTOR('',#17822,1.);
#5161=VECTOR('',#17823,1.);
#5162=VECTOR('',#17826,1.);
#5163=VECTOR('',#17827,1.);
#5164=VECTOR('',#17828,1.);
#5165=VECTOR('',#17831,1.);
#5166=VECTOR('',#17832,1.);
#5167=VECTOR('',#17845,0.5);
#5168=VECTOR('',#17852,1.05);
#5169=VECTOR('',#17859,1.05);
#5170=VECTOR('',#17864,1.);
#5171=VECTOR('',#17865,1.);
#5172=VECTOR('',#17866,1.);
#5173=VECTOR('',#17867,1.);
#5174=VECTOR('',#17870,1.);
#5175=VECTOR('',#17871,1.);
#5176=VECTOR('',#17872,1.);
#5177=VECTOR('',#17875,1.);
#5178=VECTOR('',#17876,1.);
#5179=VECTOR('',#17877,1.);
#5180=VECTOR('',#17880,1.);
#5181=VECTOR('',#17881,1.);
#5182=VECTOR('',#17892,1.04);
#5183=VECTOR('',#17903,1.04);
#5184=VECTOR('',#17914,0.65);
#5185=VECTOR('',#17921,0.8);
#5186=VECTOR('',#17926,0.8);
#5187=VECTOR('',#17929,1.);
#5188=VECTOR('',#17930,1.);
#5189=VECTOR('',#17931,1.);
#5190=VECTOR('',#17932,1.);
#5191=VECTOR('',#17935,1.);
#5192=VECTOR('',#17936,1.);
#5193=VECTOR('',#17937,1.);
#5194=VECTOR('',#17940,1.);
#5195=VECTOR('',#17941,1.);
#5196=VECTOR('',#17942,1.);
#5197=VECTOR('',#17945,1.);
#5198=VECTOR('',#17946,1.);
#5199=VECTOR('',#17957,1.04);
#5200=VECTOR('',#17968,1.04);
#5201=VECTOR('',#17979,0.65);
#5202=VECTOR('',#17984,0.8);
#5203=VECTOR('',#17989,0.8);
#5204=VECTOR('',#17994,1.);
#5205=VECTOR('',#17995,1.);
#5206=VECTOR('',#17996,1.);
#5207=VECTOR('',#17997,1.);
#5208=VECTOR('',#18000,1.);
#5209=VECTOR('',#18001,1.);
#5210=VECTOR('',#18002,1.);
#5211=VECTOR('',#18005,1.);
#5212=VECTOR('',#18006,1.);
#5213=VECTOR('',#18007,1.);
#5214=VECTOR('',#18010,1.);
#5215=VECTOR('',#18011,1.);
#5216=VECTOR('',#18020,1.);
#5217=VECTOR('',#18027,0.165);
#5218=VECTOR('',#18034,1.);
#5219=VECTOR('',#18039,0.604999999999997);
#5220=VECTOR('',#18044,1.);
#5221=VECTOR('',#18045,1.);
#5222=VECTOR('',#18046,1.);
#5223=VECTOR('',#18047,1.);
#5224=VECTOR('',#18050,1.);
#5225=VECTOR('',#18051,1.);
#5226=VECTOR('',#18052,1.);
#5227=VECTOR('',#18055,1.);
#5228=VECTOR('',#18056,1.);
#5229=VECTOR('',#18057,1.);
#5230=VECTOR('',#18060,1.);
#5231=VECTOR('',#18061,1.);
#5232=VECTOR('',#18072,0.164999999999999);
#5233=VECTOR('',#18081,0.164999999999999);
#5234=VECTOR('',#18090,0.600000000000001);
#5235=VECTOR('',#18103,0.225000000000001);
#5236=VECTOR('',#18110,1.);
#5237=VECTOR('',#18123,0.225000000000001);
#5238=VECTOR('',#18130,1.);
#5239=VECTOR('',#18143,0.604999999999997);
#5240=VECTOR('',#18150,0.799999999999997);
#5241=VECTOR('',#18163,0.604999999999997);
#5242=VECTOR('',#18170,0.799999999999997);
#5243=VECTOR('',#18183,0.604999999999997);
#5244=VECTOR('',#18190,0.799999999999997);
#5245=VECTOR('',#18203,0.604999999999997);
#5246=VECTOR('',#18210,0.799999999999997);
#5247=VECTOR('',#18225,0.65);
#5248=VECTOR('',#18232,1.05);
#5249=VECTOR('',#18239,1.05);
#5250=VECTOR('',#18244,1.);
#5251=VECTOR('',#18245,1.);
#5252=VECTOR('',#18246,1.);
#5253=VECTOR('',#18247,1.);
#5254=VECTOR('',#18250,1.);
#5255=VECTOR('',#18251,1.);
#5256=VECTOR('',#18252,1.);
#5257=VECTOR('',#18255,1.);
#5258=VECTOR('',#18256,1.);
#5259=VECTOR('',#18257,1.);
#5260=VECTOR('',#18260,1.);
#5261=VECTOR('',#18261,1.);
#5262=VECTOR('',#18272,1.04);
#5263=VECTOR('',#18283,1.04);
#5264=VECTOR('',#18294,0.65);
#5265=VECTOR('',#18301,0.800000000000001);
#5266=VECTOR('',#18306,0.800000000000001);
#5267=VECTOR('',#18309,1.);
#5268=VECTOR('',#18310,1.);
#5269=VECTOR('',#18311,1.);
#5270=VECTOR('',#18312,1.);
#5271=VECTOR('',#18315,1.);
#5272=VECTOR('',#18316,1.);
#5273=VECTOR('',#18317,1.);
#5274=VECTOR('',#18320,1.);
#5275=VECTOR('',#18321,1.);
#5276=VECTOR('',#18322,1.);
#5277=VECTOR('',#18325,1.);
#5278=VECTOR('',#18326,1.);
#5279=VECTOR('',#18337,1.04);
#5280=VECTOR('',#18348,1.04);
#5281=VECTOR('',#18359,0.65);
#5282=VECTOR('',#18364,0.800000000000001);
#5283=VECTOR('',#18369,0.800000000000001);
#5284=VECTOR('',#18374,1.);
#5285=VECTOR('',#18375,1.);
#5286=VECTOR('',#18376,1.);
#5287=VECTOR('',#18377,1.);
#5288=VECTOR('',#18380,1.);
#5289=VECTOR('',#18381,1.);
#5290=VECTOR('',#18382,1.);
#5291=VECTOR('',#18385,1.);
#5292=VECTOR('',#18386,1.);
#5293=VECTOR('',#18387,1.);
#5294=VECTOR('',#18390,1.);
#5295=VECTOR('',#18391,1.);
#5296=VECTOR('',#18400,1.);
#5297=VECTOR('',#18407,0.164999999999999);
#5298=VECTOR('',#18414,1.);
#5299=VECTOR('',#18419,0.604999999999997);
#5300=VECTOR('',#18424,1.);
#5301=VECTOR('',#18425,1.);
#5302=VECTOR('',#18426,1.);
#5303=VECTOR('',#18427,1.);
#5304=VECTOR('',#18430,1.);
#5305=VECTOR('',#18431,1.);
#5306=VECTOR('',#18432,1.);
#5307=VECTOR('',#18435,1.);
#5308=VECTOR('',#18436,1.);
#5309=VECTOR('',#18437,1.);
#5310=VECTOR('',#18440,1.);
#5311=VECTOR('',#18441,1.);
#5312=VECTOR('',#18452,0.164999999999999);
#5313=VECTOR('',#18461,0.164999999999999);
#5314=VECTOR('',#18470,0.600000000000001);
#5315=VECTOR('',#18483,0.225000000000001);
#5316=VECTOR('',#18490,1.);
#5317=VECTOR('',#18503,0.225000000000001);
#5318=VECTOR('',#18510,1.);
#5319=VECTOR('',#18523,0.604999999999997);
#5320=VECTOR('',#18530,0.799999999999997);
#5321=VECTOR('',#18543,0.604999999999997);
#5322=VECTOR('',#18550,0.799999999999997);
#5323=VECTOR('',#18563,0.604999999999997);
#5324=VECTOR('',#18570,0.799999999999997);
#5325=VECTOR('',#18583,0.604999999999997);
#5326=VECTOR('',#18590,0.799999999999997);
#5327=VECTOR('',#18605,1.);
#5328=VECTOR('',#18606,1.);
#5329=VECTOR('',#18607,1.);
#5330=VECTOR('',#18610,1.);
#5331=VECTOR('',#18611,1.);
#5332=VECTOR('',#18612,1.);
#5333=VECTOR('',#18617,1.);
#5334=VECTOR('',#18618,1.);
#5335=VECTOR('',#18621,1.);
#5336=VECTOR('',#18622,1.);
#5337=VECTOR('',#18635,1.05);
#5338=VECTOR('',#18644,1.);
#5339=VECTOR('',#18653,1.05);
#5340=VECTOR('',#18662,1.);
#5341=VECTOR('',#18671,1.05);
#5342=VECTOR('',#18678,0.9);
#5343=VECTOR('',#18685,1.);
#5344=VECTOR('',#18688,1.);
#5345=VECTOR('',#18691,1.);
#5346=VECTOR('',#18692,1.);
#5347=VECTOR('',#18693,1.);
#5348=VECTOR('',#18700,1.);
#5349=VECTOR('',#18703,1.);
#5350=VECTOR('',#18704,1.);
#5351=VECTOR('',#18715,0.895);
#5352=VECTOR('',#18722,0.605);
#5353=VECTOR('',#18735,1.);
#5354=VECTOR('',#18736,1.);
#5355=VECTOR('',#18737,1.);
#5356=VECTOR('',#18738,1.);
#5357=VECTOR('',#18741,1.);
#5358=VECTOR('',#18742,1.);
#5359=VECTOR('',#18743,1.);
#5360=VECTOR('',#18746,1.);
#5361=VECTOR('',#18747,1.);
#5362=VECTOR('',#18748,1.);
#5363=VECTOR('',#18751,1.);
#5364=VECTOR('',#18752,1.);
#5365=VECTOR('',#18753,1.);
#5366=VECTOR('',#18756,1.);
#5367=VECTOR('',#18757,1.);
#5368=VECTOR('',#18758,1.);
#5369=VECTOR('',#18761,1.);
#5370=VECTOR('',#18762,1.);
#5371=VECTOR('',#18773,0.185);
#5372=VECTOR('',#18776,0.2);
#5373=VECTOR('',#18785,1.);
#5374=VECTOR('',#18790,1.);
#5375=VECTOR('',#18793,1.);
#5376=VECTOR('',#18798,1.);
#5377=VECTOR('',#18801,1.);
#5378=VECTOR('',#18806,1.);
#5379=VECTOR('',#18807,1.);
#5380=VECTOR('',#18808,1.);
#5381=VECTOR('',#18811,1.);
#5382=VECTOR('',#18812,1.);
#5383=VECTOR('',#18813,1.);
#5384=VECTOR('',#18816,1.);
#5385=VECTOR('',#18817,1.);
#5386=VECTOR('',#18818,1.);
#5387=VECTOR('',#18823,1.);
#5388=VECTOR('',#18834,1.);
#5389=VECTOR('',#18841,1.);
#5390=VECTOR('',#18842,1.);
#5391=VECTOR('',#18845,1.);
#5392=VECTOR('',#18860,0.605);
#5393=VECTOR('',#18867,1.);
#5394=VECTOR('',#18880,0.604999999999997);
#5395=VECTOR('',#18887,1.);
#5396=VECTOR('',#18900,0.605);
#5397=VECTOR('',#18907,1.);
#5398=VECTOR('',#18920,1.);
#5399=VECTOR('',#18925,1.);
#5400=VECTOR('',#18928,1.);
#5401=VECTOR('',#18933,1.);
#5402=VECTOR('',#18936,1.);
#5403=VECTOR('',#18941,1.);
#5404=VECTOR('',#18942,1.);
#5405=VECTOR('',#18943,1.);
#5406=VECTOR('',#18946,1.);
#5407=VECTOR('',#18947,1.);
#5408=VECTOR('',#18948,1.);
#5409=VECTOR('',#18951,1.);
#5410=VECTOR('',#18952,1.);
#5411=VECTOR('',#18953,1.);
#5412=VECTOR('',#18958,1.);
#5413=VECTOR('',#18969,1.);
#5414=VECTOR('',#18976,1.);
#5415=VECTOR('',#18977,1.);
#5416=VECTOR('',#18980,1.);
#5417=VECTOR('',#18995,0.605);
#5418=VECTOR('',#19002,1.);
#5419=VECTOR('',#19015,0.604999999999997);
#5420=VECTOR('',#19022,1.);
#5421=VECTOR('',#19035,0.605);
#5422=VECTOR('',#19042,1.);
#5423=VECTOR('',#19055,0.164999999999999);
#5424=VECTOR('',#19064,0.164999999999999);
#5425=VECTOR('',#19073,0.600000000000001);
#5426=VECTOR('',#19086,0.225000000000001);
#5427=VECTOR('',#19093,1.);
#5428=VECTOR('',#19106,0.225000000000001);
#5429=VECTOR('',#19113,1.);
#5430=VECTOR('',#19126,0.605);
#5431=VECTOR('',#19133,0.800000000000001);
#5432=VECTOR('',#19146,0.605);
#5433=VECTOR('',#19153,0.800000000000001);
#5434=VECTOR('',#19166,0.605);
#5435=VECTOR('',#19173,0.800000000000001);
#5436=VECTOR('',#19186,0.605);
#5437=VECTOR('',#19193,0.800000000000001);
#5438=VECTOR('',#19206,0.605);
#5439=VECTOR('',#19213,0.800000000000001);
#5440=VECTOR('',#19230,0.325);
#5441=VECTOR('',#19235,0.35);
#5442=VECTOR('',#19240,0.335);
#5443=VECTOR('',#19249,0.21);
#5444=VECTOR('',#19254,0.2);
#5445=VECTOR('',#19259,0.18);
#5446=VECTOR('',#19264,1.);
#5447=VECTOR('',#19265,1.);
#5448=VECTOR('',#19266,1.);
#5449=VECTOR('',#19267,1.);
#5450=VECTOR('',#19270,1.);
#5451=VECTOR('',#19271,1.);
#5452=VECTOR('',#19272,1.);
#5453=VECTOR('',#19275,1.);
#5454=VECTOR('',#19276,1.);
#5455=VECTOR('',#19277,1.);
#5456=VECTOR('',#19280,1.);
#5457=VECTOR('',#19281,1.);
#5458=VECTOR('',#19282,1.);
#5459=VECTOR('',#19285,1.);
#5460=VECTOR('',#19286,1.);
#5461=VECTOR('',#19287,1.);
#5462=VECTOR('',#19290,1.);
#5463=VECTOR('',#19291,1.);
#5464=VECTOR('',#19448,0.164999999999999);
#5465=VECTOR('',#19455,0.164999999999999);
#5466=VECTOR('',#19462,0.164999999999999);
#5467=VECTOR('',#19469,0.164999999999999);
#5468=VECTOR('',#19476,1.6);
#5469=VECTOR('',#19481,1.);
#5470=VECTOR('',#19484,1.);
#5471=VECTOR('',#19489,1.);
#5472=VECTOR('',#19492,1.);
#5473=VECTOR('',#19497,1.);
#5474=VECTOR('',#19498,1.);
#5475=VECTOR('',#19499,1.);
#5476=VECTOR('',#19504,1.);
#5477=VECTOR('',#19505,1.);
#5478=VECTOR('',#19508,1.);
#5479=VECTOR('',#19515,1.);
#5480=VECTOR('',#19516,1.);
#5481=VECTOR('',#19521,1.);
#5482=VECTOR('',#19524,1.);
#5483=VECTOR('',#19527,1.);
#5484=VECTOR('',#19530,1.);
#5485=VECTOR('',#19535,1.);
#5486=VECTOR('',#19542,1.);
#5487=VECTOR('',#19551,0.604999999999997);
#5488=VECTOR('',#19558,1.);
#5489=VECTOR('',#19571,0.605);
#5490=VECTOR('',#19578,1.);
#5491=VECTOR('',#19591,0.225000000000001);
#5492=VECTOR('',#19598,0.225000000000001);
#5493=VECTOR('',#19605,0.225000000000001);
#5494=VECTOR('',#19612,0.225000000000001);
#5495=VECTOR('',#19619,1.02);
#5496=VECTOR('',#19626,2.2);
#5497=VECTOR('',#19643,0.350000000000001);
#5498=VECTOR('',#19652,0.199999999999999);
#5499=VECTOR('',#19665,0.350000000000001);
#5500=VECTOR('',#19674,0.199999999999999);
#5501=VECTOR('',#19687,0.350000000000001);
#5502=VECTOR('',#19696,0.199999999999999);
#5503=VECTOR('',#19709,0.350000000000001);
#5504=VECTOR('',#19718,0.199999999999999);
#5505=VECTOR('',#19727,0.225000000000001);
#5506=VECTOR('',#19734,0.225000000000001);
#5507=VECTOR('',#19741,0.225000000000001);
#5508=VECTOR('',#19748,0.225000000000001);
#5509=VECTOR('',#19755,1.02);
#5510=VECTOR('',#19762,2.2);
#5511=VECTOR('',#19781,0.350000000000001);
#5512=VECTOR('',#19786,0.199999999999999);
#5513=VECTOR('',#19803,0.350000000000001);
#5514=VECTOR('',#19808,0.199999999999999);
#5515=VECTOR('',#19825,0.350000000000001);
#5516=VECTOR('',#19830,0.199999999999999);
#5517=VECTOR('',#19847,0.350000000000001);
#5518=VECTOR('',#19852,0.199999999999999);
#5519=VECTOR('',#19863,0.164999999999999);
#5520=VECTOR('',#19870,0.164999999999999);
#5521=VECTOR('',#19877,0.164999999999999);
#5522=VECTOR('',#19884,0.164999999999999);
#5523=VECTOR('',#19891,1.6);
#5524=VECTOR('',#19896,1.);
#5525=VECTOR('',#19899,1.);
#5526=VECTOR('',#19904,1.);
#5527=VECTOR('',#19907,1.);
#5528=VECTOR('',#19912,1.);
#5529=VECTOR('',#19913,1.);
#5530=VECTOR('',#19914,1.);
#5531=VECTOR('',#19919,1.);
#5532=VECTOR('',#19920,1.);
#5533=VECTOR('',#19923,1.);
#5534=VECTOR('',#19930,1.);
#5535=VECTOR('',#19931,1.);
#5536=VECTOR('',#19936,1.);
#5537=VECTOR('',#19939,1.);
#5538=VECTOR('',#19942,1.);
#5539=VECTOR('',#19945,1.);
#5540=VECTOR('',#19950,1.);
#5541=VECTOR('',#19957,1.);
#5542=VECTOR('',#19966,0.604999999999997);
#5543=VECTOR('',#19973,1.);
#5544=VECTOR('',#19986,0.605);
#5545=VECTOR('',#19993,1.);
#5546=VECTOR('',#20006,0.225000000000001);
#5547=VECTOR('',#20013,0.225000000000001);
#5548=VECTOR('',#20020,0.225000000000001);
#5549=VECTOR('',#20027,0.225000000000001);
#5550=VECTOR('',#20034,1.02);
#5551=VECTOR('',#20041,2.2);
#5552=VECTOR('',#20058,0.350000000000001);
#5553=VECTOR('',#20067,0.199999999999999);
#5554=VECTOR('',#20080,0.350000000000001);
#5555=VECTOR('',#20089,0.199999999999999);
#5556=VECTOR('',#20102,0.350000000000001);
#5557=VECTOR('',#20111,0.199999999999999);
#5558=VECTOR('',#20124,0.350000000000001);
#5559=VECTOR('',#20133,0.199999999999999);
#5560=VECTOR('',#20142,0.225000000000001);
#5561=VECTOR('',#20149,0.225000000000001);
#5562=VECTOR('',#20156,0.225000000000001);
#5563=VECTOR('',#20163,0.225000000000001);
#5564=VECTOR('',#20170,1.02);
#5565=VECTOR('',#20177,2.2);
#5566=VECTOR('',#20196,0.350000000000001);
#5567=VECTOR('',#20201,0.199999999999999);
#5568=VECTOR('',#20218,0.350000000000001);
#5569=VECTOR('',#20223,0.199999999999999);
#5570=VECTOR('',#20240,0.350000000000001);
#5571=VECTOR('',#20245,0.199999999999999);
#5572=VECTOR('',#20262,0.350000000000001);
#5573=VECTOR('',#20267,0.199999999999999);
#5574=VECTOR('',#20290,1.070235);
#5575=VECTOR('',#20297,0.6);
#5576=VECTOR('',#20302,0.63);
#5577=VECTOR('',#20311,1.070235);
#5578=VECTOR('',#20318,0.63);
#5579=VECTOR('',#20337,1.129765);
#5580=VECTOR('',#20348,1.57);
#5581=VECTOR('',#20353,1.6);
#5582=VECTOR('',#20358,1.57);
#5583=VECTOR('',#20363,1.129765);
#5584=VECTOR('',#20604,1.119765);
#5585=VECTOR('',#20611,1.085235);
#5586=VECTOR('',#20622,1.119765);
#5587=VECTOR('',#20629,1.085235);
#5588=VECTOR('',#20804,0.8);
#5589=VECTOR('',#20807,0.6);
#5590=VECTOR('',#20822,0.8);
#5591=VECTOR('',#20825,0.6);
#5592=VECTOR('',#20832,0.6);
#5593=VECTOR('',#20843,0.605);
#5594=VECTOR('',#20850,0.8);
#5595=VECTOR('',#20863,0.605);
#5596=VECTOR('',#20870,0.8);
#5597=VECTOR('',#20883,0.6);
#5598=VECTOR('',#20890,0.9);
#5599=VECTOR('',#20903,0.6);
#5600=VECTOR('',#20910,0.9);
#5601=VECTOR('',#20923,0.4);
#5602=VECTOR('',#20932,0.6);
#5603=VECTOR('',#20939,2.);
#5604=CIRCLE('',#14589,0.210000000000001);
#5605=CIRCLE('',#14590,0.210000000000001);
#5606=CIRCLE('',#14592,0.210000000000001);
#5607=CIRCLE('',#14593,0.210000000000001);
#5608=CIRCLE('',#14595,0.210000000000001);
#5609=CIRCLE('',#14596,0.210000000000001);
#5610=CIRCLE('',#14598,0.210000000000001);
#5611=CIRCLE('',#14599,0.210000000000001);
#5612=CIRCLE('',#14601,0.21);
#5613=CIRCLE('',#14602,0.21);
#5614=CIRCLE('',#14604,0.21);
#5615=CIRCLE('',#14605,0.21);
#5616=CIRCLE('',#14607,0.21);
#5617=CIRCLE('',#14608,0.21);
#5618=CIRCLE('',#14610,0.21);
#5619=CIRCLE('',#14611,0.21);
#5620=CIRCLE('',#14634,0.165);
#5621=CIRCLE('',#14635,0.165);
#5622=CIRCLE('',#14637,0.165);
#5623=CIRCLE('',#14638,0.165);
#5624=CIRCLE('',#14640,0.165);
#5625=CIRCLE('',#14641,0.165);
#5626=CIRCLE('',#14643,0.165);
#5627=CIRCLE('',#14644,0.165);
#5628=CIRCLE('',#14646,1.6);
#5629=CIRCLE('',#14647,1.6);
#5630=CIRCLE('',#14649,0.275);
#5631=CIRCLE('',#14650,0.275);
#5632=CIRCLE('',#14652,0.275);
#5633=CIRCLE('',#14653,0.275);
#5634=CIRCLE('',#14655,0.275);
#5635=CIRCLE('',#14656,0.275);
#5636=CIRCLE('',#14658,0.275);
#5637=CIRCLE('',#14659,0.275);
#5638=CIRCLE('',#14665,0.605);
#5639=CIRCLE('',#14667,0.605);
#5640=CIRCLE('',#14668,0.605);
#5641=CIRCLE('',#14670,0.605);
#5642=CIRCLE('',#14672,0.605);
#5643=CIRCLE('',#14674,0.605);
#5644=CIRCLE('',#14681,0.225);
#5645=CIRCLE('',#14682,0.225);
#5646=CIRCLE('',#14684,0.225);
#5647=CIRCLE('',#14685,0.225);
#5648=CIRCLE('',#14687,0.225);
#5649=CIRCLE('',#14688,0.225);
#5650=CIRCLE('',#14690,0.225);
#5651=CIRCLE('',#14691,0.225);
#5652=CIRCLE('',#14693,1.59);
#5653=CIRCLE('',#14694,1.59);
#5654=CIRCLE('',#14696,1.02);
#5655=CIRCLE('',#14698,1.02);
#5656=CIRCLE('',#14700,2.2);
#5657=CIRCLE('',#14701,2.2);
#5658=CIRCLE('',#14706,0.225);
#5659=CIRCLE('',#14707,0.225);
#5660=CIRCLE('',#14709,0.225);
#5661=CIRCLE('',#14710,0.225);
#5662=CIRCLE('',#14712,0.225);
#5663=CIRCLE('',#14713,0.225);
#5664=CIRCLE('',#14715,0.225);
#5665=CIRCLE('',#14716,0.225);
#5666=CIRCLE('',#14718,1.59);
#5667=CIRCLE('',#14719,1.59);
#5668=CIRCLE('',#14721,1.02);
#5669=CIRCLE('',#14723,1.02);
#5670=CIRCLE('',#14725,2.2);
#5671=CIRCLE('',#14726,2.2);
#5672=CIRCLE('',#14731,0.165);
#5673=CIRCLE('',#14732,0.165);
#5674=CIRCLE('',#14734,0.165);
#5675=CIRCLE('',#14735,0.165);
#5676=CIRCLE('',#14737,0.165);
#5677=CIRCLE('',#14738,0.165);
#5678=CIRCLE('',#14740,0.165);
#5679=CIRCLE('',#14741,0.165);
#5680=CIRCLE('',#14743,1.6);
#5681=CIRCLE('',#14744,1.6);
#5682=CIRCLE('',#14746,0.274999999999999);
#5683=CIRCLE('',#14747,0.274999999999999);
#5684=CIRCLE('',#14749,0.274999999999999);
#5685=CIRCLE('',#14750,0.274999999999999);
#5686=CIRCLE('',#14752,0.274999999999999);
#5687=CIRCLE('',#14753,0.274999999999999);
#5688=CIRCLE('',#14755,0.274999999999999);
#5689=CIRCLE('',#14756,0.274999999999999);
#5690=CIRCLE('',#14763,0.605);
#5691=CIRCLE('',#14764,0.605);
#5692=CIRCLE('',#14766,0.605);
#5693=CIRCLE('',#14768,0.605);
#5694=CIRCLE('',#14775,0.225);
#5695=CIRCLE('',#14776,0.225);
#5696=CIRCLE('',#14778,0.225);
#5697=CIRCLE('',#14779,0.225);
#5698=CIRCLE('',#14781,0.225);
#5699=CIRCLE('',#14782,0.225);
#5700=CIRCLE('',#14784,0.225);
#5701=CIRCLE('',#14785,0.225);
#5702=CIRCLE('',#14787,1.59);
#5703=CIRCLE('',#14788,1.59);
#5704=CIRCLE('',#14790,1.02);
#5705=CIRCLE('',#14792,1.02);
#5706=CIRCLE('',#14794,2.2);
#5707=CIRCLE('',#14795,2.2);
#5708=CIRCLE('',#14800,0.225);
#5709=CIRCLE('',#14801,0.225);
#5710=CIRCLE('',#14803,0.225);
#5711=CIRCLE('',#14804,0.225);
#5712=CIRCLE('',#14806,0.225);
#5713=CIRCLE('',#14807,0.225);
#5714=CIRCLE('',#14809,0.225);
#5715=CIRCLE('',#14810,0.225);
#5716=CIRCLE('',#14812,1.59);
#5717=CIRCLE('',#14813,1.59);
#5718=CIRCLE('',#14815,1.02);
#5719=CIRCLE('',#14817,1.02);
#5720=CIRCLE('',#14819,2.2);
#5721=CIRCLE('',#14820,2.2);
#5722=CIRCLE('',#14825,0.6);
#5723=CIRCLE('',#14826,0.6);
#5724=CIRCLE('',#14831,0.6);
#5725=CIRCLE('',#14832,0.6);
#5726=CIRCLE('',#14837,0.165);
#5727=CIRCLE('',#14838,0.165);
#5728=CIRCLE('',#14841,0.165);
#5729=CIRCLE('',#14842,0.165);
#5730=CIRCLE('',#14845,0.6);
#5731=CIRCLE('',#14846,0.6);
#5732=CIRCLE('',#14851,0.225);
#5733=CIRCLE('',#14852,0.225);
#5734=CIRCLE('',#14854,1.);
#5735=CIRCLE('',#14855,1.);
#5736=CIRCLE('',#14860,0.225);
#5737=CIRCLE('',#14861,0.225);
#5738=CIRCLE('',#14863,1.);
#5739=CIRCLE('',#14864,1.);
#5740=CIRCLE('',#14869,0.605);
#5741=CIRCLE('',#14870,0.605);
#5742=CIRCLE('',#14872,0.8);
#5743=CIRCLE('',#14873,0.8);
#5744=CIRCLE('',#14878,0.605);
#5745=CIRCLE('',#14879,0.605);
#5746=CIRCLE('',#14881,0.8);
#5747=CIRCLE('',#14882,0.8);
#5748=CIRCLE('',#14887,0.605);
#5749=CIRCLE('',#14888,0.605);
#5750=CIRCLE('',#14890,0.8);
#5751=CIRCLE('',#14891,0.8);
#5752=CIRCLE('',#14904,0.1954);
#5753=CIRCLE('',#14906,0.3);
#5754=CIRCLE('',#14908,0.35);
#5755=CIRCLE('',#14910,0.35);
#5756=CIRCLE('',#14912,0.32);
#5757=CIRCLE('',#14914,0.22);
#5758=CIRCLE('',#14916,0.1954);
#5759=CIRCLE('',#14921,0.274999999999999);
#5760=CIRCLE('',#14922,0.274999999999999);
#5761=CIRCLE('',#14924,0.274999999999999);
#5762=CIRCLE('',#14925,0.274999999999999);
#5763=CIRCLE('',#14927,0.274999999999999);
#5764=CIRCLE('',#14928,0.274999999999999);
#5765=CIRCLE('',#14930,0.274999999999999);
#5766=CIRCLE('',#14931,0.274999999999999);
#5767=CIRCLE('',#14933,0.275);
#5768=CIRCLE('',#14934,0.275);
#5769=CIRCLE('',#14936,0.275);
#5770=CIRCLE('',#14937,0.275);
#5771=CIRCLE('',#14939,0.275);
#5772=CIRCLE('',#14940,0.275);
#5773=CIRCLE('',#14942,0.275);
#5774=CIRCLE('',#14943,0.275);
#5775=CIRCLE('',#14952,0.21);
#5776=CIRCLE('',#14953,0.21);
#5777=CIRCLE('',#14955,0.21);
#5778=CIRCLE('',#14956,0.21);
#5779=CIRCLE('',#14958,0.21);
#5780=CIRCLE('',#14959,0.21);
#5781=CIRCLE('',#14961,0.21);
#5782=CIRCLE('',#14962,0.21);
#5783=CIRCLE('',#14969,0.605);
#5784=CIRCLE('',#14971,0.605);
#5785=CIRCLE('',#14972,0.605);
#5786=CIRCLE('',#14974,0.605);
#5787=CIRCLE('',#14976,0.605);
#5788=CIRCLE('',#14978,0.605);
#5789=CIRCLE('',#14985,0.210000000000001);
#5790=CIRCLE('',#14986,0.210000000000001);
#5791=CIRCLE('',#14988,0.210000000000001);
#5792=CIRCLE('',#14989,0.210000000000001);
#5793=CIRCLE('',#14991,0.210000000000001);
#5794=CIRCLE('',#14992,0.210000000000001);
#5795=CIRCLE('',#14994,0.210000000000001);
#5796=CIRCLE('',#14995,0.210000000000001);
#5797=CIRCLE('',#15001,0.605);
#5798=CIRCLE('',#15002,0.605);
#5799=CIRCLE('',#15005,0.605);
#5800=CIRCLE('',#15007,0.605);
#5801=CIRCLE('',#15014,0.6);
#5802=CIRCLE('',#15015,0.6);
#5803=CIRCLE('',#15020,0.6);
#5804=CIRCLE('',#15021,0.6);
#5805=CIRCLE('',#15026,0.165);
#5806=CIRCLE('',#15027,0.165);
#5807=CIRCLE('',#15030,0.165);
#5808=CIRCLE('',#15031,0.165);
#5809=CIRCLE('',#15034,0.6);
#5810=CIRCLE('',#15035,0.6);
#5811=CIRCLE('',#15040,0.225);
#5812=CIRCLE('',#15041,0.225);
#5813=CIRCLE('',#15043,1.);
#5814=CIRCLE('',#15044,1.);
#5815=CIRCLE('',#15049,0.225);
#5816=CIRCLE('',#15050,0.225);
#5817=CIRCLE('',#15052,1.);
#5818=CIRCLE('',#15053,1.);
#5819=CIRCLE('',#15058,0.605);
#5820=CIRCLE('',#15059,0.605);
#5821=CIRCLE('',#15061,0.8);
#5822=CIRCLE('',#15062,0.8);
#5823=CIRCLE('',#15067,0.605);
#5824=CIRCLE('',#15068,0.605);
#5825=CIRCLE('',#15070,0.8);
#5826=CIRCLE('',#15071,0.8);
#5827=CIRCLE('',#15076,0.605);
#5828=CIRCLE('',#15077,0.605);
#5829=CIRCLE('',#15079,0.8);
#5830=CIRCLE('',#15080,0.8);
#5831=CIRCLE('',#15085,0.605);
#5832=CIRCLE('',#15086,0.605);
#5833=CIRCLE('',#15088,0.8);
#5834=CIRCLE('',#15089,0.8);
#5835=CIRCLE('',#15094,0.375);
#5836=CIRCLE('',#15096,0.425);
#5837=CIRCLE('',#15098,0.425);
#5838=CIRCLE('',#15100,0.395);
#5839=CIRCLE('',#15102,0.27);
#5840=CIRCLE('',#15104,0.24505);
#5841=CIRCLE('',#15106,0.24505);
#5842=CIRCLE('',#15108,0.2);
#5843=CIRCLE('',#15121,0.5);
#5844=CIRCLE('',#15122,0.5);
#5845=CIRCLE('',#15124,1.05);
#5846=CIRCLE('',#15125,1.05);
#5847=CIRCLE('',#15127,1.05);
#5848=CIRCLE('',#15128,1.05);
#5849=CIRCLE('',#15137,1.04);
#5850=CIRCLE('',#15138,1.04);
#5851=CIRCLE('',#15140,0.8);
#5852=CIRCLE('',#15142,1.04);
#5853=CIRCLE('',#15143,1.04);
#5854=CIRCLE('',#15145,0.8);
#5855=CIRCLE('',#15147,0.65);
#5856=CIRCLE('',#15148,0.65);
#5857=CIRCLE('',#15150,0.8);
#5858=CIRCLE('',#15152,0.8);
#5859=CIRCLE('',#15161,1.04);
#5860=CIRCLE('',#15162,1.04);
#5861=CIRCLE('',#15164,0.8);
#5862=CIRCLE('',#15166,1.04);
#5863=CIRCLE('',#15167,1.04);
#5864=CIRCLE('',#15169,0.8);
#5865=CIRCLE('',#15171,0.65);
#5866=CIRCLE('',#15172,0.65);
#5867=CIRCLE('',#15174,0.8);
#5868=CIRCLE('',#15176,0.8);
#5869=CIRCLE('',#15185,0.165);
#5870=CIRCLE('',#15187,0.165);
#5871=CIRCLE('',#15188,0.165);
#5872=CIRCLE('',#15189,0.165);
#5873=CIRCLE('',#15192,0.604999999999997);
#5874=CIRCLE('',#15193,0.604999999999997);
#5875=CIRCLE('',#15202,0.164999999999999);
#5876=CIRCLE('',#15203,0.164999999999999);
#5877=CIRCLE('',#15206,0.164999999999999);
#5878=CIRCLE('',#15207,0.164999999999999);
#5879=CIRCLE('',#15210,0.600000000000001);
#5880=CIRCLE('',#15211,0.600000000000001);
#5881=CIRCLE('',#15216,0.225000000000001);
#5882=CIRCLE('',#15217,0.225000000000001);
#5883=CIRCLE('',#15219,1.);
#5884=CIRCLE('',#15220,1.);
#5885=CIRCLE('',#15225,0.225000000000001);
#5886=CIRCLE('',#15226,0.225000000000001);
#5887=CIRCLE('',#15228,1.);
#5888=CIRCLE('',#15229,1.);
#5889=CIRCLE('',#15234,0.604999999999997);
#5890=CIRCLE('',#15235,0.604999999999997);
#5891=CIRCLE('',#15237,0.799999999999997);
#5892=CIRCLE('',#15238,0.799999999999997);
#5893=CIRCLE('',#15243,0.604999999999997);
#5894=CIRCLE('',#15244,0.604999999999997);
#5895=CIRCLE('',#15246,0.799999999999997);
#5896=CIRCLE('',#15247,0.799999999999997);
#5897=CIRCLE('',#15252,0.604999999999997);
#5898=CIRCLE('',#15253,0.604999999999997);
#5899=CIRCLE('',#15255,0.799999999999997);
#5900=CIRCLE('',#15256,0.799999999999997);
#5901=CIRCLE('',#15261,0.604999999999997);
#5902=CIRCLE('',#15262,0.604999999999997);
#5903=CIRCLE('',#15264,0.799999999999997);
#5904=CIRCLE('',#15265,0.799999999999997);
#5905=CIRCLE('',#15271,0.65);
#5906=CIRCLE('',#15272,0.65);
#5907=CIRCLE('',#15274,1.05);
#5908=CIRCLE('',#15275,1.05);
#5909=CIRCLE('',#15277,1.05);
#5910=CIRCLE('',#15278,1.05);
#5911=CIRCLE('',#15287,1.04);
#5912=CIRCLE('',#15288,1.04);
#5913=CIRCLE('',#15290,0.800000000000001);
#5914=CIRCLE('',#15292,1.04);
#5915=CIRCLE('',#15293,1.04);
#5916=CIRCLE('',#15295,0.800000000000001);
#5917=CIRCLE('',#15297,0.65);
#5918=CIRCLE('',#15298,0.65);
#5919=CIRCLE('',#15300,0.800000000000001);
#5920=CIRCLE('',#15302,0.800000000000001);
#5921=CIRCLE('',#15311,1.04);
#5922=CIRCLE('',#15312,1.04);
#5923=CIRCLE('',#15314,0.800000000000001);
#5924=CIRCLE('',#15316,1.04);
#5925=CIRCLE('',#15317,1.04);
#5926=CIRCLE('',#15319,0.800000000000001);
#5927=CIRCLE('',#15321,0.65);
#5928=CIRCLE('',#15322,0.65);
#5929=CIRCLE('',#15324,0.800000000000001);
#5930=CIRCLE('',#15326,0.800000000000001);
#5931=CIRCLE('',#15335,0.164999999999999);
#5932=CIRCLE('',#15337,0.164999999999999);
#5933=CIRCLE('',#15338,0.164999999999999);
#5934=CIRCLE('',#15339,0.164999999999999);
#5935=CIRCLE('',#15342,0.604999999999997);
#5936=CIRCLE('',#15343,0.604999999999997);
#5937=CIRCLE('',#15352,0.164999999999999);
#5938=CIRCLE('',#15353,0.164999999999999);
#5939=CIRCLE('',#15356,0.164999999999999);
#5940=CIRCLE('',#15357,0.164999999999999);
#5941=CIRCLE('',#15360,0.600000000000001);
#5942=CIRCLE('',#15361,0.600000000000001);
#5943=CIRCLE('',#15366,0.225000000000001);
#5944=CIRCLE('',#15367,0.225000000000001);
#5945=CIRCLE('',#15369,1.);
#5946=CIRCLE('',#15370,1.);
#5947=CIRCLE('',#15375,0.225000000000001);
#5948=CIRCLE('',#15376,0.225000000000001);
#5949=CIRCLE('',#15378,1.);
#5950=CIRCLE('',#15379,1.);
#5951=CIRCLE('',#15384,0.604999999999997);
#5952=CIRCLE('',#15385,0.604999999999997);
#5953=CIRCLE('',#15387,0.799999999999997);
#5954=CIRCLE('',#15388,0.799999999999997);
#5955=CIRCLE('',#15393,0.604999999999997);
#5956=CIRCLE('',#15394,0.604999999999997);
#5957=CIRCLE('',#15396,0.799999999999997);
#5958=CIRCLE('',#15397,0.799999999999997);
#5959=CIRCLE('',#15402,0.604999999999997);
#5960=CIRCLE('',#15403,0.604999999999997);
#5961=CIRCLE('',#15405,0.799999999999997);
#5962=CIRCLE('',#15406,0.799999999999997);
#5963=CIRCLE('',#15411,0.604999999999997);
#5964=CIRCLE('',#15412,0.604999999999997);
#5965=CIRCLE('',#15414,0.799999999999997);
#5966=CIRCLE('',#15415,0.799999999999997);
#5967=CIRCLE('',#15421,0.9);
#5968=CIRCLE('',#15424,0.9);
#5969=CIRCLE('',#15428,1.05);
#5970=CIRCLE('',#15429,0.9);
#5971=CIRCLE('',#15431,1.05);
#5972=CIRCLE('',#15433,1.);
#5973=CIRCLE('',#15435,1.);
#5974=CIRCLE('',#15437,1.05);
#5975=CIRCLE('',#15439,1.05);
#5976=CIRCLE('',#15441,1.);
#5977=CIRCLE('',#15443,1.);
#5978=CIRCLE('',#15445,1.05);
#5979=CIRCLE('',#15447,1.05);
#5980=CIRCLE('',#15449,0.9);
#5981=CIRCLE('',#15453,0.895);
#5982=CIRCLE('',#15454,0.605);
#5983=CIRCLE('',#15457,0.895);
#5984=CIRCLE('',#15458,0.605);
#5985=CIRCLE('',#15461,0.895);
#5986=CIRCLE('',#15462,0.605);
#5987=CIRCLE('',#15464,0.895);
#5988=CIRCLE('',#15466,0.605);
#5989=CIRCLE('',#15472,0.1954);
#5990=CIRCLE('',#15481,0.17);
#5991=CIRCLE('',#15483,0.1954);
#5992=CIRCLE('',#15488,1.);
#5993=CIRCLE('',#15489,1.);
#5994=CIRCLE('',#15491,1.5);
#5995=CIRCLE('',#15492,1.5);
#5996=CIRCLE('',#15494,1.5);
#5997=CIRCLE('',#15495,1.5);
#5998=CIRCLE('',#15500,1.);
#5999=CIRCLE('',#15501,1.);
#6000=CIRCLE('',#15503,1.5);
#6001=CIRCLE('',#15504,1.5);
#6002=CIRCLE('',#15506,1.5);
#6003=CIRCLE('',#15507,1.);
#6004=CIRCLE('',#15510,1.);
#6005=CIRCLE('',#15512,1.5);
#6006=CIRCLE('',#15516,0.605);
#6007=CIRCLE('',#15517,0.605);
#6008=CIRCLE('',#15519,1.);
#6009=CIRCLE('',#15520,1.);
#6010=CIRCLE('',#15525,0.604999999999997);
#6011=CIRCLE('',#15526,0.604999999999997);
#6012=CIRCLE('',#15528,1.);
#6013=CIRCLE('',#15529,1.);
#6014=CIRCLE('',#15534,0.605);
#6015=CIRCLE('',#15535,0.605);
#6016=CIRCLE('',#15537,1.);
#6017=CIRCLE('',#15538,1.);
#6018=CIRCLE('',#15543,1.);
#6019=CIRCLE('',#15544,1.);
#6020=CIRCLE('',#15546,1.5);
#6021=CIRCLE('',#15547,1.5);
#6022=CIRCLE('',#15549,1.5);
#6023=CIRCLE('',#15550,1.5);
#6024=CIRCLE('',#15555,1.);
#6025=CIRCLE('',#15556,1.);
#6026=CIRCLE('',#15558,1.5);
#6027=CIRCLE('',#15559,1.5);
#6028=CIRCLE('',#15561,1.5);
#6029=CIRCLE('',#15562,1.);
#6030=CIRCLE('',#15565,1.);
#6031=CIRCLE('',#15567,1.5);
#6032=CIRCLE('',#15571,0.605);
#6033=CIRCLE('',#15572,0.605);
#6034=CIRCLE('',#15574,1.);
#6035=CIRCLE('',#15575,1.);
#6036=CIRCLE('',#15580,0.604999999999997);
#6037=CIRCLE('',#15581,0.604999999999997);
#6038=CIRCLE('',#15583,1.);
#6039=CIRCLE('',#15584,1.);
#6040=CIRCLE('',#15589,0.605);
#6041=CIRCLE('',#15590,0.605);
#6042=CIRCLE('',#15592,1.);
#6043=CIRCLE('',#15593,1.);
#6044=CIRCLE('',#15598,0.164999999999999);
#6045=CIRCLE('',#15599,0.164999999999999);
#6046=CIRCLE('',#15602,0.164999999999999);
#6047=CIRCLE('',#15603,0.164999999999999);
#6048=CIRCLE('',#15606,0.600000000000001);
#6049=CIRCLE('',#15607,0.600000000000001);
#6050=CIRCLE('',#15612,0.225000000000001);
#6051=CIRCLE('',#15613,0.225000000000001);
#6052=CIRCLE('',#15615,1.);
#6053=CIRCLE('',#15616,1.);
#6054=CIRCLE('',#15621,0.225000000000001);
#6055=CIRCLE('',#15622,0.225000000000001);
#6056=CIRCLE('',#15624,1.);
#6057=CIRCLE('',#15625,1.);
#6058=CIRCLE('',#15630,0.605);
#6059=CIRCLE('',#15631,0.605);
#6060=CIRCLE('',#15633,0.800000000000001);
#6061=CIRCLE('',#15634,0.800000000000001);
#6062=CIRCLE('',#15639,0.605);
#6063=CIRCLE('',#15640,0.605);
#6064=CIRCLE('',#15642,0.800000000000001);
#6065=CIRCLE('',#15643,0.800000000000001);
#6066=CIRCLE('',#15648,0.605);
#6067=CIRCLE('',#15649,0.605);
#6068=CIRCLE('',#15651,0.800000000000001);
#6069=CIRCLE('',#15652,0.800000000000001);
#6070=CIRCLE('',#15657,0.605);
#6071=CIRCLE('',#15658,0.605);
#6072=CIRCLE('',#15660,0.800000000000001);
#6073=CIRCLE('',#15661,0.800000000000001);
#6074=CIRCLE('',#15666,0.605);
#6075=CIRCLE('',#15667,0.605);
#6076=CIRCLE('',#15669,0.800000000000001);
#6077=CIRCLE('',#15670,0.800000000000001);
#6078=CIRCLE('',#15675,0.3);
#6079=CIRCLE('',#15677,0.35);
#6080=CIRCLE('',#15679,0.35);
#6081=CIRCLE('',#15681,0.32);
#6082=CIRCLE('',#15683,0.22);
#6083=CIRCLE('',#15685,0.1954);
#6084=CIRCLE('',#15687,0.1954);
#6085=CIRCLE('',#15689,0.16);
#6086=CIRCLE('',#15774,0.164999999999999);
#6087=CIRCLE('',#15775,0.164999999999999);
#6088=CIRCLE('',#15777,0.164999999999999);
#6089=CIRCLE('',#15778,0.164999999999999);
#6090=CIRCLE('',#15780,0.164999999999999);
#6091=CIRCLE('',#15781,0.164999999999999);
#6092=CIRCLE('',#15783,0.164999999999999);
#6093=CIRCLE('',#15784,0.164999999999999);
#6094=CIRCLE('',#15786,1.6);
#6095=CIRCLE('',#15787,1.6);
#6096=CIRCLE('',#15789,2.2);
#6097=CIRCLE('',#15790,2.2);
#6098=CIRCLE('',#15792,2.2);
#6099=CIRCLE('',#15793,2.2);
#6100=CIRCLE('',#15796,1.5);
#6101=CIRCLE('',#15797,1.5);
#6102=CIRCLE('',#15798,1.);
#6103=CIRCLE('',#15799,1.);
#6104=CIRCLE('',#15802,1.);
#6105=CIRCLE('',#15804,1.5);
#6106=CIRCLE('',#15807,1.);
#6107=CIRCLE('',#15809,1.5);
#6108=CIRCLE('',#15814,0.604999999999997);
#6109=CIRCLE('',#15815,0.604999999999997);
#6110=CIRCLE('',#15817,1.);
#6111=CIRCLE('',#15818,1.);
#6112=CIRCLE('',#15823,0.605);
#6113=CIRCLE('',#15824,0.605);
#6114=CIRCLE('',#15826,1.);
#6115=CIRCLE('',#15827,1.);
#6116=CIRCLE('',#15832,0.225000000000001);
#6117=CIRCLE('',#15833,0.225000000000001);
#6118=CIRCLE('',#15835,0.225000000000001);
#6119=CIRCLE('',#15836,0.225000000000001);
#6120=CIRCLE('',#15838,0.225000000000001);
#6121=CIRCLE('',#15839,0.225000000000001);
#6122=CIRCLE('',#15841,0.225000000000001);
#6123=CIRCLE('',#15842,0.225000000000001);
#6124=CIRCLE('',#15844,1.02);
#6125=CIRCLE('',#15845,1.02);
#6126=CIRCLE('',#15847,2.2);
#6127=CIRCLE('',#15848,2.2);
#6128=CIRCLE('',#15853,0.350000000000001);
#6129=CIRCLE('',#15854,0.199999999999999);
#6130=CIRCLE('',#15856,0.350000000000001);
#6131=CIRCLE('',#15859,0.199999999999999);
#6132=CIRCLE('',#15863,0.350000000000001);
#6133=CIRCLE('',#15864,0.199999999999999);
#6134=CIRCLE('',#15866,0.350000000000001);
#6135=CIRCLE('',#15869,0.199999999999999);
#6136=CIRCLE('',#15873,0.350000000000001);
#6137=CIRCLE('',#15874,0.199999999999999);
#6138=CIRCLE('',#15876,0.350000000000001);
#6139=CIRCLE('',#15879,0.199999999999999);
#6140=CIRCLE('',#15883,0.350000000000001);
#6141=CIRCLE('',#15884,0.199999999999999);
#6142=CIRCLE('',#15886,0.350000000000001);
#6143=CIRCLE('',#15889,0.199999999999999);
#6144=CIRCLE('',#15893,0.225000000000001);
#6145=CIRCLE('',#15894,0.225000000000001);
#6146=CIRCLE('',#15896,0.225000000000001);
#6147=CIRCLE('',#15897,0.225000000000001);
#6148=CIRCLE('',#15899,0.225000000000001);
#6149=CIRCLE('',#15900,0.225000000000001);
#6150=CIRCLE('',#15902,0.225000000000001);
#6151=CIRCLE('',#15903,0.225000000000001);
#6152=CIRCLE('',#15905,1.02);
#6153=CIRCLE('',#15906,1.02);
#6154=CIRCLE('',#15908,2.2);
#6155=CIRCLE('',#15909,2.2);
#6156=CIRCLE('',#15914,0.350000000000001);
#6157=CIRCLE('',#15915,0.199999999999999);
#6158=CIRCLE('',#15917,0.350000000000001);
#6159=CIRCLE('',#15920,0.199999999999999);
#6160=CIRCLE('',#15924,0.350000000000001);
#6161=CIRCLE('',#15925,0.199999999999999);
#6162=CIRCLE('',#15927,0.350000000000001);
#6163=CIRCLE('',#15930,0.199999999999999);
#6164=CIRCLE('',#15934,0.350000000000001);
#6165=CIRCLE('',#15935,0.199999999999999);
#6166=CIRCLE('',#15937,0.350000000000001);
#6167=CIRCLE('',#15940,0.199999999999999);
#6168=CIRCLE('',#15944,0.350000000000001);
#6169=CIRCLE('',#15945,0.199999999999999);
#6170=CIRCLE('',#15947,0.350000000000001);
#6171=CIRCLE('',#15950,0.199999999999999);
#6172=CIRCLE('',#15954,0.164999999999999);
#6173=CIRCLE('',#15955,0.164999999999999);
#6174=CIRCLE('',#15957,0.164999999999999);
#6175=CIRCLE('',#15958,0.164999999999999);
#6176=CIRCLE('',#15960,0.164999999999999);
#6177=CIRCLE('',#15961,0.164999999999999);
#6178=CIRCLE('',#15963,0.164999999999999);
#6179=CIRCLE('',#15964,0.164999999999999);
#6180=CIRCLE('',#15966,1.6);
#6181=CIRCLE('',#15967,1.6);
#6182=CIRCLE('',#15969,2.2);
#6183=CIRCLE('',#15970,2.2);
#6184=CIRCLE('',#15972,2.2);
#6185=CIRCLE('',#15973,2.2);
#6186=CIRCLE('',#15976,1.5);
#6187=CIRCLE('',#15977,1.5);
#6188=CIRCLE('',#15978,1.);
#6189=CIRCLE('',#15979,1.);
#6190=CIRCLE('',#15982,1.);
#6191=CIRCLE('',#15984,1.5);
#6192=CIRCLE('',#15987,1.);
#6193=CIRCLE('',#15989,1.5);
#6194=CIRCLE('',#15994,0.604999999999997);
#6195=CIRCLE('',#15995,0.604999999999997);
#6196=CIRCLE('',#15997,1.);
#6197=CIRCLE('',#15998,1.);
#6198=CIRCLE('',#16003,0.605);
#6199=CIRCLE('',#16004,0.605);
#6200=CIRCLE('',#16006,1.);
#6201=CIRCLE('',#16007,1.);
#6202=CIRCLE('',#16012,0.225000000000001);
#6203=CIRCLE('',#16013,0.225000000000001);
#6204=CIRCLE('',#16015,0.225000000000001);
#6205=CIRCLE('',#16016,0.225000000000001);
#6206=CIRCLE('',#16018,0.225000000000001);
#6207=CIRCLE('',#16019,0.225000000000001);
#6208=CIRCLE('',#16021,0.225000000000001);
#6209=CIRCLE('',#16022,0.225000000000001);
#6210=CIRCLE('',#16024,1.02);
#6211=CIRCLE('',#16025,1.02);
#6212=CIRCLE('',#16027,2.2);
#6213=CIRCLE('',#16028,2.2);
#6214=CIRCLE('',#16033,0.350000000000001);
#6215=CIRCLE('',#16034,0.199999999999999);
#6216=CIRCLE('',#16036,0.350000000000001);
#6217=CIRCLE('',#16039,0.199999999999999);
#6218=CIRCLE('',#16043,0.350000000000001);
#6219=CIRCLE('',#16044,0.199999999999999);
#6220=CIRCLE('',#16046,0.350000000000001);
#6221=CIRCLE('',#16049,0.199999999999999);
#6222=CIRCLE('',#16053,0.350000000000001);
#6223=CIRCLE('',#16054,0.199999999999999);
#6224=CIRCLE('',#16056,0.350000000000001);
#6225=CIRCLE('',#16059,0.199999999999999);
#6226=CIRCLE('',#16063,0.350000000000001);
#6227=CIRCLE('',#16064,0.199999999999999);
#6228=CIRCLE('',#16066,0.350000000000001);
#6229=CIRCLE('',#16069,0.199999999999999);
#6230=CIRCLE('',#16073,0.225000000000001);
#6231=CIRCLE('',#16074,0.225000000000001);
#6232=CIRCLE('',#16076,0.225000000000001);
#6233=CIRCLE('',#16077,0.225000000000001);
#6234=CIRCLE('',#16079,0.225000000000001);
#6235=CIRCLE('',#16080,0.225000000000001);
#6236=CIRCLE('',#16082,0.225000000000001);
#6237=CIRCLE('',#16083,0.225000000000001);
#6238=CIRCLE('',#16085,1.02);
#6239=CIRCLE('',#16086,1.02);
#6240=CIRCLE('',#16088,2.2);
#6241=CIRCLE('',#16089,2.2);
#6242=CIRCLE('',#16094,0.350000000000001);
#6243=CIRCLE('',#16095,0.199999999999999);
#6244=CIRCLE('',#16097,0.350000000000001);
#6245=CIRCLE('',#16100,0.199999999999999);
#6246=CIRCLE('',#16104,0.350000000000001);
#6247=CIRCLE('',#16105,0.199999999999999);
#6248=CIRCLE('',#16107,0.350000000000001);
#6249=CIRCLE('',#16110,0.199999999999999);
#6250=CIRCLE('',#16114,0.350000000000001);
#6251=CIRCLE('',#16115,0.199999999999999);
#6252=CIRCLE('',#16117,0.350000000000001);
#6253=CIRCLE('',#16120,0.199999999999999);
#6254=CIRCLE('',#16124,0.350000000000001);
#6255=CIRCLE('',#16125,0.199999999999999);
#6256=CIRCLE('',#16127,0.350000000000001);
#6257=CIRCLE('',#16130,0.199999999999999);
#6258=CIRCLE('',#16135,1.070235);
#6259=CIRCLE('',#16136,1.070235);
#6260=CIRCLE('',#16137,0.309556);
#6261=CIRCLE('',#16138,1.070235);
#6262=CIRCLE('',#16139,1.070235);
#6263=CIRCLE('',#16141,1.070235);
#6264=CIRCLE('',#16143,0.6);
#6265=CIRCLE('',#16144,0.6);
#6266=CIRCLE('',#16146,0.66);
#6267=CIRCLE('',#16149,1.070235);
#6268=CIRCLE('',#16151,0.66);
#6269=CIRCLE('',#16155,1.129765);
#6270=CIRCLE('',#16156,1.129765);
#6271=CIRCLE('',#16157,0.309556);
#6272=CIRCLE('',#16158,1.129765);
#6273=CIRCLE('',#16159,1.129765);
#6274=CIRCLE('',#16161,1.129765);
#6275=CIRCLE('',#16163,1.54);
#6276=CIRCLE('',#16164,1.129765);
#6277=CIRCLE('',#16166,1.6);
#6278=CIRCLE('',#16168,1.6);
#6279=CIRCLE('',#16170,1.54);
#6280=CIRCLE('',#16175,0.29765);
#6281=CIRCLE('',#16177,0.29765);
#6282=CIRCLE('',#16179,0.29765);
#6283=CIRCLE('',#16181,0.29765);
#6284=CIRCLE('',#16183,0.29765);
#6285=CIRCLE('',#16185,0.29765);
#6286=CIRCLE('',#16187,0.29765);
#6287=CIRCLE('',#16190,0.267289037081583);
#6288=CIRCLE('',#16191,0.226018648221778);
#6289=CIRCLE('',#16193,1.308355);
#6290=CIRCLE('',#16194,0.226018648221778);
#6291=CIRCLE('',#16195,0.891645);
#6292=CIRCLE('',#16197,1.308355);
#6293=CIRCLE('',#16199,0.891645);
#6294=CIRCLE('',#16200,0.267289037081583);
#6295=CIRCLE('',#16204,0.226018648221778);
#6296=CIRCLE('',#16205,0.267289037081583);
#6297=CIRCLE('',#16207,0.891645);
#6298=CIRCLE('',#16208,0.267289037081583);
#6299=CIRCLE('',#16209,1.308355);
#6300=CIRCLE('',#16211,1.308355);
#6301=CIRCLE('',#16213,0.891645);
#6302=CIRCLE('',#16215,0.226018648221778);
#6303=CIRCLE('',#16218,0.267289037081583);
#6304=CIRCLE('',#16219,0.226018648221778);
#6305=CIRCLE('',#16221,1.308355);
#6306=CIRCLE('',#16222,1.308355);
#6307=CIRCLE('',#16224,0.226018648221778);
#6308=CIRCLE('',#16225,0.891645);
#6309=CIRCLE('',#16227,0.891645);
#6310=CIRCLE('',#16228,0.267289037081583);
#6311=CIRCLE('',#16232,0.267289037081583);
#6312=CIRCLE('',#16233,0.226018648221778);
#6313=CIRCLE('',#16235,1.308355);
#6314=CIRCLE('',#16236,1.308355);
#6315=CIRCLE('',#16238,0.891645);
#6316=CIRCLE('',#16239,0.226018648221778);
#6317=CIRCLE('',#16241,0.891645);
#6318=CIRCLE('',#16243,0.267289037081583);
#6319=CIRCLE('',#16246,0.226018648221778);
#6320=CIRCLE('',#16247,0.267289037081583);
#6321=CIRCLE('',#16249,0.891645);
#6322=CIRCLE('',#16250,0.891645);
#6323=CIRCLE('',#16252,0.267289037081583);
#6324=CIRCLE('',#16253,1.308355);
#6325=CIRCLE('',#16255,0.226018648221778);
#6326=CIRCLE('',#16256,1.308355);
#6327=CIRCLE('',#16260,0.226018648221778);
#6328=CIRCLE('',#16261,0.267289037081583);
#6329=CIRCLE('',#16263,0.891645);
#6330=CIRCLE('',#16264,0.891645);
#6331=CIRCLE('',#16266,0.267289037081583);
#6332=CIRCLE('',#16267,1.308355);
#6333=CIRCLE('',#16269,1.308355);
#6334=CIRCLE('',#16271,0.226018648221778);
#6335=CIRCLE('',#16274,1.308355);
#6336=CIRCLE('',#16275,1.308355);
#6337=CIRCLE('',#16277,0.226018648221778);
#6338=CIRCLE('',#16278,0.226018648221778);
#6339=CIRCLE('',#16279,0.891645);
#6340=CIRCLE('',#16281,0.267289037081583);
#6341=CIRCLE('',#16283,0.267289037081583);
#6342=CIRCLE('',#16284,0.891645);
#6343=CIRCLE('',#16289,1.119765);
#6344=CIRCLE('',#16290,1.085235);
#6345=CIRCLE('',#16292,1.119765);
#6346=CIRCLE('',#16294,1.085235);
#6347=CIRCLE('',#16297,1.119765);
#6348=CIRCLE('',#16298,1.085235);
#6349=CIRCLE('',#16300,1.119765);
#6350=CIRCLE('',#16302,1.085235);
#6351=CIRCLE('',#16385,0.8);
#6352=CIRCLE('',#16386,0.6);
#6353=CIRCLE('',#16388,0.8);
#6354=CIRCLE('',#16389,0.6);
#6355=CIRCLE('',#16392,0.6);
#6356=CIRCLE('',#16394,0.8);
#6357=CIRCLE('',#16396,0.8);
#6358=CIRCLE('',#16397,0.6);
#6359=CIRCLE('',#16400,0.6);
#6360=CIRCLE('',#16402,0.6);
#6361=CIRCLE('',#16407,0.605);
#6362=CIRCLE('',#16408,0.605);
#6363=CIRCLE('',#16410,0.8);
#6364=CIRCLE('',#16411,0.8);
#6365=CIRCLE('',#16416,0.605);
#6366=CIRCLE('',#16417,0.605);
#6367=CIRCLE('',#16419,0.8);
#6368=CIRCLE('',#16420,0.8);
#6369=CIRCLE('',#16425,0.6);
#6370=CIRCLE('',#16426,0.6);
#6371=CIRCLE('',#16428,0.9);
#6372=CIRCLE('',#16429,0.9);
#6373=CIRCLE('',#16434,0.6);
#6374=CIRCLE('',#16435,0.6);
#6375=CIRCLE('',#16437,0.9);
#6376=CIRCLE('',#16438,0.9);
#6377=CIRCLE('',#16443,0.4);
#6378=CIRCLE('',#16444,0.4);
#6379=CIRCLE('',#16447,0.6);
#6380=CIRCLE('',#16448,0.6);
#6381=CIRCLE('',#16450,2.);
#6382=CIRCLE('',#16451,2.);
#6383=VERTEX_POINT('',#20978);
#6384=VERTEX_POINT('',#20980);
#6385=VERTEX_POINT('',#20984);
#6386=VERTEX_POINT('',#20986);
#6387=VERTEX_POINT('',#20990);
#6388=VERTEX_POINT('',#20992);
#6389=VERTEX_POINT('',#20996);
#6390=VERTEX_POINT('',#20998);
#6391=VERTEX_POINT('',#21002);
#6392=VERTEX_POINT('',#21004);
#6393=VERTEX_POINT('',#21008);
#6394=VERTEX_POINT('',#21010);
#6395=VERTEX_POINT('',#21014);
#6396=VERTEX_POINT('',#21016);
#6397=VERTEX_POINT('',#21020);
#6398=VERTEX_POINT('',#21022);
#6399=VERTEX_POINT('',#21026);
#6400=VERTEX_POINT('',#21027);
#6401=VERTEX_POINT('',#21029);
#6402=VERTEX_POINT('',#21031);
#6403=VERTEX_POINT('',#21035);
#6404=VERTEX_POINT('',#21037);
#6405=VERTEX_POINT('',#21041);
#6406=VERTEX_POINT('',#21043);
#6407=VERTEX_POINT('',#21053);
#6408=VERTEX_POINT('',#21054);
#6409=VERTEX_POINT('',#21056);
#6410=VERTEX_POINT('',#21058);
#6411=VERTEX_POINT('',#21062);
#6412=VERTEX_POINT('',#21064);
#6413=VERTEX_POINT('',#21068);
#6414=VERTEX_POINT('',#21070);
#6415=VERTEX_POINT('',#21080);
#6416=VERTEX_POINT('',#21081);
#6417=VERTEX_POINT('',#21083);
#6418=VERTEX_POINT('',#21085);
#6419=VERTEX_POINT('',#21089);
#6420=VERTEX_POINT('',#21091);
#6421=VERTEX_POINT('',#21095);
#6422=VERTEX_POINT('',#21097);
#6423=VERTEX_POINT('',#21107);
#6424=VERTEX_POINT('',#21109);
#6425=VERTEX_POINT('',#21113);
#6426=VERTEX_POINT('',#21115);
#6427=VERTEX_POINT('',#21119);
#6428=VERTEX_POINT('',#21121);
#6429=VERTEX_POINT('',#21125);
#6430=VERTEX_POINT('',#21127);
#6431=VERTEX_POINT('',#21131);
#6432=VERTEX_POINT('',#21133);
#6433=VERTEX_POINT('',#21137);
#6434=VERTEX_POINT('',#21139);
#6435=VERTEX_POINT('',#21143);
#6436=VERTEX_POINT('',#21145);
#6437=VERTEX_POINT('',#21149);
#6438=VERTEX_POINT('',#21151);
#6439=VERTEX_POINT('',#21155);
#6440=VERTEX_POINT('',#21157);
#6441=VERTEX_POINT('',#21161);
#6442=VERTEX_POINT('',#21162);
#6443=VERTEX_POINT('',#21164);
#6444=VERTEX_POINT('',#21166);
#6445=VERTEX_POINT('',#21170);
#6446=VERTEX_POINT('',#21171);
#6447=VERTEX_POINT('',#21173);
#6448=VERTEX_POINT('',#21175);
#6449=VERTEX_POINT('',#21179);
#6450=VERTEX_POINT('',#21180);
#6451=VERTEX_POINT('',#21185);
#6452=VERTEX_POINT('',#21186);
#6453=VERTEX_POINT('',#21191);
#6454=VERTEX_POINT('',#21193);
#6455=VERTEX_POINT('',#21197);
#6456=VERTEX_POINT('',#21200);
#6457=VERTEX_POINT('',#21203);
#6458=VERTEX_POINT('',#21205);
#6459=VERTEX_POINT('',#21208);
#6460=VERTEX_POINT('',#21212);
#6461=VERTEX_POINT('',#21216);
#6462=VERTEX_POINT('',#21220);
#6463=VERTEX_POINT('',#21230);
#6464=VERTEX_POINT('',#21232);
#6465=VERTEX_POINT('',#21236);
#6466=VERTEX_POINT('',#21238);
#6467=VERTEX_POINT('',#21242);
#6468=VERTEX_POINT('',#21244);
#6469=VERTEX_POINT('',#21248);
#6470=VERTEX_POINT('',#21250);
#6471=VERTEX_POINT('',#21254);
#6472=VERTEX_POINT('',#21256);
#6473=VERTEX_POINT('',#21260);
#6474=VERTEX_POINT('',#21263);
#6475=VERTEX_POINT('',#21267);
#6476=VERTEX_POINT('',#21269);
#6477=VERTEX_POINT('',#21276);
#6478=VERTEX_POINT('',#21278);
#6479=VERTEX_POINT('',#21282);
#6480=VERTEX_POINT('',#21284);
#6481=VERTEX_POINT('',#21288);
#6482=VERTEX_POINT('',#21290);
#6483=VERTEX_POINT('',#21294);
#6484=VERTEX_POINT('',#21296);
#6485=VERTEX_POINT('',#21300);
#6486=VERTEX_POINT('',#21302);
#6487=VERTEX_POINT('',#21306);
#6488=VERTEX_POINT('',#21309);
#6489=VERTEX_POINT('',#21313);
#6490=VERTEX_POINT('',#21315);
#6491=VERTEX_POINT('',#21322);
#6492=VERTEX_POINT('',#21324);
#6493=VERTEX_POINT('',#21328);
#6494=VERTEX_POINT('',#21330);
#6495=VERTEX_POINT('',#21334);
#6496=VERTEX_POINT('',#21336);
#6497=VERTEX_POINT('',#21340);
#6498=VERTEX_POINT('',#21342);
#6499=VERTEX_POINT('',#21346);
#6500=VERTEX_POINT('',#21348);
#6501=VERTEX_POINT('',#21352);
#6502=VERTEX_POINT('',#21354);
#6503=VERTEX_POINT('',#21358);
#6504=VERTEX_POINT('',#21360);
#6505=VERTEX_POINT('',#21364);
#6506=VERTEX_POINT('',#21366);
#6507=VERTEX_POINT('',#21370);
#6508=VERTEX_POINT('',#21372);
#6509=VERTEX_POINT('',#21376);
#6510=VERTEX_POINT('',#21377);
#6511=VERTEX_POINT('',#21379);
#6512=VERTEX_POINT('',#21381);
#6513=VERTEX_POINT('',#21385);
#6514=VERTEX_POINT('',#21386);
#6515=VERTEX_POINT('',#21388);
#6516=VERTEX_POINT('',#21390);
#6517=VERTEX_POINT('',#21394);
#6518=VERTEX_POINT('',#21395);
#6519=VERTEX_POINT('',#21400);
#6520=VERTEX_POINT('',#21401);
#6521=VERTEX_POINT('',#21406);
#6522=VERTEX_POINT('',#21408);
#6523=VERTEX_POINT('',#21413);
#6524=VERTEX_POINT('',#21416);
#6525=VERTEX_POINT('',#21418);
#6526=VERTEX_POINT('',#21421);
#6527=VERTEX_POINT('',#21425);
#6528=VERTEX_POINT('',#21429);
#6529=VERTEX_POINT('',#21439);
#6530=VERTEX_POINT('',#21441);
#6531=VERTEX_POINT('',#21445);
#6532=VERTEX_POINT('',#21447);
#6533=VERTEX_POINT('',#21451);
#6534=VERTEX_POINT('',#21453);
#6535=VERTEX_POINT('',#21457);
#6536=VERTEX_POINT('',#21459);
#6537=VERTEX_POINT('',#21463);
#6538=VERTEX_POINT('',#21465);
#6539=VERTEX_POINT('',#21469);
#6540=VERTEX_POINT('',#21472);
#6541=VERTEX_POINT('',#21476);
#6542=VERTEX_POINT('',#21478);
#6543=VERTEX_POINT('',#21485);
#6544=VERTEX_POINT('',#21487);
#6545=VERTEX_POINT('',#21491);
#6546=VERTEX_POINT('',#21493);
#6547=VERTEX_POINT('',#21497);
#6548=VERTEX_POINT('',#21499);
#6549=VERTEX_POINT('',#21503);
#6550=VERTEX_POINT('',#21505);
#6551=VERTEX_POINT('',#21509);
#6552=VERTEX_POINT('',#21511);
#6553=VERTEX_POINT('',#21515);
#6554=VERTEX_POINT('',#21518);
#6555=VERTEX_POINT('',#21522);
#6556=VERTEX_POINT('',#21524);
#6557=VERTEX_POINT('',#21531);
#6558=VERTEX_POINT('',#21533);
#6559=VERTEX_POINT('',#21540);
#6560=VERTEX_POINT('',#21542);
#6561=VERTEX_POINT('',#21549);
#6562=VERTEX_POINT('',#21551);
#6563=VERTEX_POINT('',#21556);
#6564=VERTEX_POINT('',#21558);
#6565=VERTEX_POINT('',#21563);
#6566=VERTEX_POINT('',#21565);
#6567=VERTEX_POINT('',#21572);
#6568=VERTEX_POINT('',#21574);
#6569=VERTEX_POINT('',#21578);
#6570=VERTEX_POINT('',#21580);
#6571=VERTEX_POINT('',#21587);
#6572=VERTEX_POINT('',#21589);
#6573=VERTEX_POINT('',#21593);
#6574=VERTEX_POINT('',#21595);
#6575=VERTEX_POINT('',#21602);
#6576=VERTEX_POINT('',#21604);
#6577=VERTEX_POINT('',#21608);
#6578=VERTEX_POINT('',#21610);
#6579=VERTEX_POINT('',#21617);
#6580=VERTEX_POINT('',#21619);
#6581=VERTEX_POINT('',#21623);
#6582=VERTEX_POINT('',#21625);
#6583=VERTEX_POINT('',#21632);
#6584=VERTEX_POINT('',#21634);
#6585=VERTEX_POINT('',#21638);
#6586=VERTEX_POINT('',#21640);
#6587=VERTEX_POINT('',#21647);
#6588=VERTEX_POINT('',#21648);
#6589=VERTEX_POINT('',#21650);
#6590=VERTEX_POINT('',#21652);
#6591=VERTEX_POINT('',#21656);
#6592=VERTEX_POINT('',#21658);
#6593=VERTEX_POINT('',#21662);
#6594=VERTEX_POINT('',#21664);
#6595=VERTEX_POINT('',#21668);
#6596=VERTEX_POINT('',#21670);
#6597=VERTEX_POINT('',#21674);
#6598=VERTEX_POINT('',#21676);
#6599=VERTEX_POINT('',#21685);
#6600=VERTEX_POINT('',#21688);
#6601=VERTEX_POINT('',#21691);
#6602=VERTEX_POINT('',#21695);
#6603=VERTEX_POINT('',#21699);
#6604=VERTEX_POINT('',#21703);
#6605=VERTEX_POINT('',#21706);
#6606=VERTEX_POINT('',#21714);
#6607=VERTEX_POINT('',#21716);
#6608=VERTEX_POINT('',#21720);
#6609=VERTEX_POINT('',#21722);
#6610=VERTEX_POINT('',#21726);
#6611=VERTEX_POINT('',#21728);
#6612=VERTEX_POINT('',#21732);
#6613=VERTEX_POINT('',#21734);
#6614=VERTEX_POINT('',#21738);
#6615=VERTEX_POINT('',#21740);
#6616=VERTEX_POINT('',#21744);
#6617=VERTEX_POINT('',#21746);
#6618=VERTEX_POINT('',#21750);
#6619=VERTEX_POINT('',#21752);
#6620=VERTEX_POINT('',#21756);
#6621=VERTEX_POINT('',#21758);
#6622=VERTEX_POINT('',#21762);
#6623=VERTEX_POINT('',#21763);
#6624=VERTEX_POINT('',#21765);
#6625=VERTEX_POINT('',#21767);
#6626=VERTEX_POINT('',#21771);
#6627=VERTEX_POINT('',#21773);
#6628=VERTEX_POINT('',#21777);
#6629=VERTEX_POINT('',#21779);
#6630=VERTEX_POINT('',#21789);
#6631=VERTEX_POINT('',#21791);
#6632=VERTEX_POINT('',#21795);
#6633=VERTEX_POINT('',#21797);
#6634=VERTEX_POINT('',#21801);
#6635=VERTEX_POINT('',#21803);
#6636=VERTEX_POINT('',#21807);
#6637=VERTEX_POINT('',#21809);
#6638=VERTEX_POINT('',#21813);
#6639=VERTEX_POINT('',#21814);
#6640=VERTEX_POINT('',#21816);
#6641=VERTEX_POINT('',#21818);
#6642=VERTEX_POINT('',#21821);
#6643=VERTEX_POINT('',#21822);
#6644=VERTEX_POINT('',#21824);
#6645=VERTEX_POINT('',#21826);
#6646=VERTEX_POINT('',#21830);
#6647=VERTEX_POINT('',#21832);
#6648=VERTEX_POINT('',#21836);
#6649=VERTEX_POINT('',#21840);
#6650=VERTEX_POINT('',#21846);
#6651=VERTEX_POINT('',#21848);
#6652=VERTEX_POINT('',#21851);
#6653=VERTEX_POINT('',#21854);
#6654=VERTEX_POINT('',#21857);
#6655=VERTEX_POINT('',#21859);
#6656=VERTEX_POINT('',#21862);
#6657=VERTEX_POINT('',#21866);
#6658=VERTEX_POINT('',#21870);
#6659=VERTEX_POINT('',#21874);
#6660=VERTEX_POINT('',#21883);
#6661=VERTEX_POINT('',#21885);
#6662=VERTEX_POINT('',#21889);
#6663=VERTEX_POINT('',#21891);
#6664=VERTEX_POINT('',#21895);
#6665=VERTEX_POINT('',#21897);
#6666=VERTEX_POINT('',#21901);
#6667=VERTEX_POINT('',#21903);
#6668=VERTEX_POINT('',#21907);
#6669=VERTEX_POINT('',#21908);
#6670=VERTEX_POINT('',#21910);
#6671=VERTEX_POINT('',#21912);
#6672=VERTEX_POINT('',#21916);
#6673=VERTEX_POINT('',#21917);
#6674=VERTEX_POINT('',#21919);
#6675=VERTEX_POINT('',#21921);
#6676=VERTEX_POINT('',#21925);
#6677=VERTEX_POINT('',#21927);
#6678=VERTEX_POINT('',#21931);
#6679=VERTEX_POINT('',#21932);
#6680=VERTEX_POINT('',#21937);
#6681=VERTEX_POINT('',#21939);
#6682=VERTEX_POINT('',#21942);
#6683=VERTEX_POINT('',#21944);
#6684=VERTEX_POINT('',#21947);
#6685=VERTEX_POINT('',#21952);
#6686=VERTEX_POINT('',#21956);
#6687=VERTEX_POINT('',#21960);
#6688=VERTEX_POINT('',#21970);
#6689=VERTEX_POINT('',#21972);
#6690=VERTEX_POINT('',#21979);
#6691=VERTEX_POINT('',#21981);
#6692=VERTEX_POINT('',#21988);
#6693=VERTEX_POINT('',#21990);
#6694=VERTEX_POINT('',#21995);
#6695=VERTEX_POINT('',#21997);
#6696=VERTEX_POINT('',#22002);
#6697=VERTEX_POINT('',#22004);
#6698=VERTEX_POINT('',#22011);
#6699=VERTEX_POINT('',#22013);
#6700=VERTEX_POINT('',#22017);
#6701=VERTEX_POINT('',#22019);
#6702=VERTEX_POINT('',#22026);
#6703=VERTEX_POINT('',#22028);
#6704=VERTEX_POINT('',#22032);
#6705=VERTEX_POINT('',#22034);
#6706=VERTEX_POINT('',#22041);
#6707=VERTEX_POINT('',#22043);
#6708=VERTEX_POINT('',#22047);
#6709=VERTEX_POINT('',#22049);
#6710=VERTEX_POINT('',#22056);
#6711=VERTEX_POINT('',#22058);
#6712=VERTEX_POINT('',#22062);
#6713=VERTEX_POINT('',#22064);
#6714=VERTEX_POINT('',#22071);
#6715=VERTEX_POINT('',#22073);
#6716=VERTEX_POINT('',#22077);
#6717=VERTEX_POINT('',#22079);
#6718=VERTEX_POINT('',#22086);
#6719=VERTEX_POINT('',#22088);
#6720=VERTEX_POINT('',#22092);
#6721=VERTEX_POINT('',#22094);
#6722=VERTEX_POINT('',#22101);
#6723=VERTEX_POINT('',#22104);
#6724=VERTEX_POINT('',#22108);
#6725=VERTEX_POINT('',#22112);
#6726=VERTEX_POINT('',#22116);
#6727=VERTEX_POINT('',#22119);
#6728=VERTEX_POINT('',#22123);
#6729=VERTEX_POINT('',#22127);
#6730=VERTEX_POINT('',#22132);
#6731=VERTEX_POINT('',#22133);
#6732=VERTEX_POINT('',#22135);
#6733=VERTEX_POINT('',#22137);
#6734=VERTEX_POINT('',#22141);
#6735=VERTEX_POINT('',#22143);
#6736=VERTEX_POINT('',#22147);
#6737=VERTEX_POINT('',#22149);
#6738=VERTEX_POINT('',#22153);
#6739=VERTEX_POINT('',#22155);
#6740=VERTEX_POINT('',#22159);
#6741=VERTEX_POINT('',#22161);
#6742=VERTEX_POINT('',#22172);
#6743=VERTEX_POINT('',#22174);
#6744=VERTEX_POINT('',#22178);
#6745=VERTEX_POINT('',#22180);
#6746=VERTEX_POINT('',#22184);
#6747=VERTEX_POINT('',#22186);
#6748=VERTEX_POINT('',#22190);
#6749=VERTEX_POINT('',#22191);
#6750=VERTEX_POINT('',#22193);
#6751=VERTEX_POINT('',#22195);
#6752=VERTEX_POINT('',#22199);
#6753=VERTEX_POINT('',#22201);
#6754=VERTEX_POINT('',#22205);
#6755=VERTEX_POINT('',#22207);
#6756=VERTEX_POINT('',#22217);
#6757=VERTEX_POINT('',#22219);
#6758=VERTEX_POINT('',#22223);
#6759=VERTEX_POINT('',#22226);
#6760=VERTEX_POINT('',#22228);
#6761=VERTEX_POINT('',#22232);
#6762=VERTEX_POINT('',#22235);
#6763=VERTEX_POINT('',#22237);
#6764=VERTEX_POINT('',#22241);
#6765=VERTEX_POINT('',#22245);
#6766=VERTEX_POINT('',#22249);
#6767=VERTEX_POINT('',#22250);
#6768=VERTEX_POINT('',#22252);
#6769=VERTEX_POINT('',#22254);
#6770=VERTEX_POINT('',#22258);
#6771=VERTEX_POINT('',#22260);
#6772=VERTEX_POINT('',#22264);
#6773=VERTEX_POINT('',#22266);
#6774=VERTEX_POINT('',#22276);
#6775=VERTEX_POINT('',#22278);
#6776=VERTEX_POINT('',#22282);
#6777=VERTEX_POINT('',#22285);
#6778=VERTEX_POINT('',#22287);
#6779=VERTEX_POINT('',#22291);
#6780=VERTEX_POINT('',#22294);
#6781=VERTEX_POINT('',#22296);
#6782=VERTEX_POINT('',#22300);
#6783=VERTEX_POINT('',#22304);
#6784=VERTEX_POINT('',#22308);
#6785=VERTEX_POINT('',#22309);
#6786=VERTEX_POINT('',#22311);
#6787=VERTEX_POINT('',#22313);
#6788=VERTEX_POINT('',#22317);
#6789=VERTEX_POINT('',#22319);
#6790=VERTEX_POINT('',#22323);
#6791=VERTEX_POINT('',#22325);
#6792=VERTEX_POINT('',#22335);
#6793=VERTEX_POINT('',#22336);
#6794=VERTEX_POINT('',#22340);
#6795=VERTEX_POINT('',#22355);
#6796=VERTEX_POINT('',#22357);
#6797=VERTEX_POINT('',#22360);
#6798=VERTEX_POINT('',#22379);
#6799=VERTEX_POINT('',#22381);
#6800=VERTEX_POINT('',#22385);
#6801=VERTEX_POINT('',#22386);
#6802=VERTEX_POINT('',#22388);
#6803=VERTEX_POINT('',#22390);
#6804=VERTEX_POINT('',#22394);
#6805=VERTEX_POINT('',#22396);
#6806=VERTEX_POINT('',#22400);
#6807=VERTEX_POINT('',#22402);
#6808=VERTEX_POINT('',#22412);
#6809=VERTEX_POINT('',#22414);
#6810=VERTEX_POINT('',#22419);
#6811=VERTEX_POINT('',#22421);
#6812=VERTEX_POINT('',#22426);
#6813=VERTEX_POINT('',#22428);
#6814=VERTEX_POINT('',#22435);
#6815=VERTEX_POINT('',#22437);
#6816=VERTEX_POINT('',#22441);
#6817=VERTEX_POINT('',#22443);
#6818=VERTEX_POINT('',#22450);
#6819=VERTEX_POINT('',#22452);
#6820=VERTEX_POINT('',#22456);
#6821=VERTEX_POINT('',#22458);
#6822=VERTEX_POINT('',#22465);
#6823=VERTEX_POINT('',#22467);
#6824=VERTEX_POINT('',#22471);
#6825=VERTEX_POINT('',#22473);
#6826=VERTEX_POINT('',#22480);
#6827=VERTEX_POINT('',#22482);
#6828=VERTEX_POINT('',#22486);
#6829=VERTEX_POINT('',#22488);
#6830=VERTEX_POINT('',#22495);
#6831=VERTEX_POINT('',#22497);
#6832=VERTEX_POINT('',#22501);
#6833=VERTEX_POINT('',#22503);
#6834=VERTEX_POINT('',#22510);
#6835=VERTEX_POINT('',#22512);
#6836=VERTEX_POINT('',#22516);
#6837=VERTEX_POINT('',#22518);
#6838=VERTEX_POINT('',#22526);
#6839=VERTEX_POINT('',#22528);
#6840=VERTEX_POINT('',#22532);
#6841=VERTEX_POINT('',#22534);
#6842=VERTEX_POINT('',#22538);
#6843=VERTEX_POINT('',#22540);
#6844=VERTEX_POINT('',#22544);
#6845=VERTEX_POINT('',#22545);
#6846=VERTEX_POINT('',#22547);
#6847=VERTEX_POINT('',#22549);
#6848=VERTEX_POINT('',#22553);
#6849=VERTEX_POINT('',#22555);
#6850=VERTEX_POINT('',#22559);
#6851=VERTEX_POINT('',#22561);
#6852=VERTEX_POINT('',#22571);
#6853=VERTEX_POINT('',#22573);
#6854=VERTEX_POINT('',#22577);
#6855=VERTEX_POINT('',#22580);
#6856=VERTEX_POINT('',#22582);
#6857=VERTEX_POINT('',#22586);
#6858=VERTEX_POINT('',#22589);
#6859=VERTEX_POINT('',#22591);
#6860=VERTEX_POINT('',#22595);
#6861=VERTEX_POINT('',#22599);
#6862=VERTEX_POINT('',#22603);
#6863=VERTEX_POINT('',#22604);
#6864=VERTEX_POINT('',#22606);
#6865=VERTEX_POINT('',#22608);
#6866=VERTEX_POINT('',#22612);
#6867=VERTEX_POINT('',#22614);
#6868=VERTEX_POINT('',#22618);
#6869=VERTEX_POINT('',#22620);
#6870=VERTEX_POINT('',#22630);
#6871=VERTEX_POINT('',#22632);
#6872=VERTEX_POINT('',#22636);
#6873=VERTEX_POINT('',#22639);
#6874=VERTEX_POINT('',#22641);
#6875=VERTEX_POINT('',#22645);
#6876=VERTEX_POINT('',#22648);
#6877=VERTEX_POINT('',#22650);
#6878=VERTEX_POINT('',#22654);
#6879=VERTEX_POINT('',#22658);
#6880=VERTEX_POINT('',#22662);
#6881=VERTEX_POINT('',#22663);
#6882=VERTEX_POINT('',#22665);
#6883=VERTEX_POINT('',#22667);
#6884=VERTEX_POINT('',#22671);
#6885=VERTEX_POINT('',#22673);
#6886=VERTEX_POINT('',#22677);
#6887=VERTEX_POINT('',#22679);
#6888=VERTEX_POINT('',#22689);
#6889=VERTEX_POINT('',#22690);
#6890=VERTEX_POINT('',#22694);
#6891=VERTEX_POINT('',#22709);
#6892=VERTEX_POINT('',#22711);
#6893=VERTEX_POINT('',#22714);
#6894=VERTEX_POINT('',#22733);
#6895=VERTEX_POINT('',#22735);
#6896=VERTEX_POINT('',#22739);
#6897=VERTEX_POINT('',#22740);
#6898=VERTEX_POINT('',#22742);
#6899=VERTEX_POINT('',#22744);
#6900=VERTEX_POINT('',#22748);
#6901=VERTEX_POINT('',#22750);
#6902=VERTEX_POINT('',#22754);
#6903=VERTEX_POINT('',#22756);
#6904=VERTEX_POINT('',#22766);
#6905=VERTEX_POINT('',#22768);
#6906=VERTEX_POINT('',#22773);
#6907=VERTEX_POINT('',#22775);
#6908=VERTEX_POINT('',#22780);
#6909=VERTEX_POINT('',#22782);
#6910=VERTEX_POINT('',#22789);
#6911=VERTEX_POINT('',#22791);
#6912=VERTEX_POINT('',#22795);
#6913=VERTEX_POINT('',#22797);
#6914=VERTEX_POINT('',#22804);
#6915=VERTEX_POINT('',#22806);
#6916=VERTEX_POINT('',#22810);
#6917=VERTEX_POINT('',#22812);
#6918=VERTEX_POINT('',#22819);
#6919=VERTEX_POINT('',#22821);
#6920=VERTEX_POINT('',#22825);
#6921=VERTEX_POINT('',#22827);
#6922=VERTEX_POINT('',#22834);
#6923=VERTEX_POINT('',#22836);
#6924=VERTEX_POINT('',#22840);
#6925=VERTEX_POINT('',#22842);
#6926=VERTEX_POINT('',#22849);
#6927=VERTEX_POINT('',#22851);
#6928=VERTEX_POINT('',#22855);
#6929=VERTEX_POINT('',#22857);
#6930=VERTEX_POINT('',#22864);
#6931=VERTEX_POINT('',#22866);
#6932=VERTEX_POINT('',#22870);
#6933=VERTEX_POINT('',#22872);
#6934=VERTEX_POINT('',#22880);
#6935=VERTEX_POINT('',#22881);
#6936=VERTEX_POINT('',#22883);
#6937=VERTEX_POINT('',#22885);
#6938=VERTEX_POINT('',#22889);
#6939=VERTEX_POINT('',#22891);
#6940=VERTEX_POINT('',#22895);
#6941=VERTEX_POINT('',#22897);
#6942=VERTEX_POINT('',#22905);
#6943=VERTEX_POINT('',#22907);
#6944=VERTEX_POINT('',#22910);
#6945=VERTEX_POINT('',#22914);
#6946=VERTEX_POINT('',#22917);
#6947=VERTEX_POINT('',#22921);
#6948=VERTEX_POINT('',#22924);
#6949=VERTEX_POINT('',#22928);
#6950=VERTEX_POINT('',#22931);
#6951=VERTEX_POINT('',#22935);
#6952=VERTEX_POINT('',#22938);
#6953=VERTEX_POINT('',#22942);
#6954=VERTEX_POINT('',#22948);
#6955=VERTEX_POINT('',#22949);
#6956=VERTEX_POINT('',#22951);
#6957=VERTEX_POINT('',#22953);
#6958=VERTEX_POINT('',#22957);
#6959=VERTEX_POINT('',#22959);
#6960=VERTEX_POINT('',#22963);
#6961=VERTEX_POINT('',#22965);
#6962=VERTEX_POINT('',#22972);
#6963=VERTEX_POINT('',#22974);
#6964=VERTEX_POINT('',#22977);
#6965=VERTEX_POINT('',#22981);
#6966=VERTEX_POINT('',#22989);
#6967=VERTEX_POINT('',#22992);
#6968=VERTEX_POINT('',#22993);
#6969=VERTEX_POINT('',#22995);
#6970=VERTEX_POINT('',#22997);
#6971=VERTEX_POINT('',#23001);
#6972=VERTEX_POINT('',#23003);
#6973=VERTEX_POINT('',#23007);
#6974=VERTEX_POINT('',#23009);
#6975=VERTEX_POINT('',#23013);
#6976=VERTEX_POINT('',#23015);
#6977=VERTEX_POINT('',#23019);
#6978=VERTEX_POINT('',#23021);
#6979=VERTEX_POINT('',#23029);
#6980=VERTEX_POINT('',#23032);
#6981=VERTEX_POINT('',#23040);
#6982=VERTEX_POINT('',#23042);
#6983=VERTEX_POINT('',#23046);
#6984=VERTEX_POINT('',#23047);
#6985=VERTEX_POINT('',#23049);
#6986=VERTEX_POINT('',#23051);
#6987=VERTEX_POINT('',#23055);
#6988=VERTEX_POINT('',#23056);
#6989=VERTEX_POINT('',#23058);
#6990=VERTEX_POINT('',#23060);
#6991=VERTEX_POINT('',#23064);
#6992=VERTEX_POINT('',#23066);
#6993=VERTEX_POINT('',#23070);
#6994=VERTEX_POINT('',#23072);
#6995=VERTEX_POINT('',#23076);
#6996=VERTEX_POINT('',#23078);
#6997=VERTEX_POINT('',#23082);
#6998=VERTEX_POINT('',#23084);
#6999=VERTEX_POINT('',#23091);
#7000=VERTEX_POINT('',#23094);
#7001=VERTEX_POINT('',#23097);
#7002=VERTEX_POINT('',#23101);
#7003=VERTEX_POINT('',#23109);
#7004=VERTEX_POINT('',#23111);
#7005=VERTEX_POINT('',#23115);
#7006=VERTEX_POINT('',#23117);
#7007=VERTEX_POINT('',#23124);
#7008=VERTEX_POINT('',#23126);
#7009=VERTEX_POINT('',#23130);
#7010=VERTEX_POINT('',#23132);
#7011=VERTEX_POINT('',#23139);
#7012=VERTEX_POINT('',#23141);
#7013=VERTEX_POINT('',#23145);
#7014=VERTEX_POINT('',#23147);
#7015=VERTEX_POINT('',#23154);
#7016=VERTEX_POINT('',#23156);
#7017=VERTEX_POINT('',#23160);
#7018=VERTEX_POINT('',#23161);
#7019=VERTEX_POINT('',#23163);
#7020=VERTEX_POINT('',#23165);
#7021=VERTEX_POINT('',#23169);
#7022=VERTEX_POINT('',#23170);
#7023=VERTEX_POINT('',#23172);
#7024=VERTEX_POINT('',#23174);
#7025=VERTEX_POINT('',#23178);
#7026=VERTEX_POINT('',#23180);
#7027=VERTEX_POINT('',#23184);
#7028=VERTEX_POINT('',#23186);
#7029=VERTEX_POINT('',#23190);
#7030=VERTEX_POINT('',#23192);
#7031=VERTEX_POINT('',#23196);
#7032=VERTEX_POINT('',#23198);
#7033=VERTEX_POINT('',#23205);
#7034=VERTEX_POINT('',#23208);
#7035=VERTEX_POINT('',#23211);
#7036=VERTEX_POINT('',#23215);
#7037=VERTEX_POINT('',#23223);
#7038=VERTEX_POINT('',#23225);
#7039=VERTEX_POINT('',#23229);
#7040=VERTEX_POINT('',#23231);
#7041=VERTEX_POINT('',#23238);
#7042=VERTEX_POINT('',#23240);
#7043=VERTEX_POINT('',#23244);
#7044=VERTEX_POINT('',#23246);
#7045=VERTEX_POINT('',#23253);
#7046=VERTEX_POINT('',#23255);
#7047=VERTEX_POINT('',#23259);
#7048=VERTEX_POINT('',#23261);
#7049=VERTEX_POINT('',#23268);
#7050=VERTEX_POINT('',#23270);
#7051=VERTEX_POINT('',#23275);
#7052=VERTEX_POINT('',#23277);
#7053=VERTEX_POINT('',#23282);
#7054=VERTEX_POINT('',#23284);
#7055=VERTEX_POINT('',#23291);
#7056=VERTEX_POINT('',#23293);
#7057=VERTEX_POINT('',#23297);
#7058=VERTEX_POINT('',#23299);
#7059=VERTEX_POINT('',#23306);
#7060=VERTEX_POINT('',#23308);
#7061=VERTEX_POINT('',#23312);
#7062=VERTEX_POINT('',#23314);
#7063=VERTEX_POINT('',#23321);
#7064=VERTEX_POINT('',#23323);
#7065=VERTEX_POINT('',#23327);
#7066=VERTEX_POINT('',#23329);
#7067=VERTEX_POINT('',#23336);
#7068=VERTEX_POINT('',#23338);
#7069=VERTEX_POINT('',#23342);
#7070=VERTEX_POINT('',#23344);
#7071=VERTEX_POINT('',#23351);
#7072=VERTEX_POINT('',#23353);
#7073=VERTEX_POINT('',#23357);
#7074=VERTEX_POINT('',#23359);
#7075=VERTEX_POINT('',#23366);
#7076=VERTEX_POINT('',#23368);
#7077=VERTEX_POINT('',#23372);
#7078=VERTEX_POINT('',#23374);
#7079=VERTEX_POINT('',#23381);
#7080=VERTEX_POINT('',#23383);
#7081=VERTEX_POINT('',#23387);
#7082=VERTEX_POINT('',#23389);
#7083=VERTEX_POINT('',#23396);
#7084=VERTEX_POINT('',#23399);
#7085=VERTEX_POINT('',#23403);
#7086=VERTEX_POINT('',#23407);
#7087=VERTEX_POINT('',#23411);
#7088=VERTEX_POINT('',#23414);
#7089=VERTEX_POINT('',#23418);
#7090=VERTEX_POINT('',#23422);
#7091=VERTEX_POINT('',#23427);
#7092=VERTEX_POINT('',#23428);
#7093=VERTEX_POINT('',#23430);
#7094=VERTEX_POINT('',#23432);
#7095=VERTEX_POINT('',#23436);
#7096=VERTEX_POINT('',#23438);
#7097=VERTEX_POINT('',#23442);
#7098=VERTEX_POINT('',#23444);
#7099=VERTEX_POINT('',#23448);
#7100=VERTEX_POINT('',#23450);
#7101=VERTEX_POINT('',#23454);
#7102=VERTEX_POINT('',#23456);
#7103=VERTEX_POINT('',#23539);
#7104=VERTEX_POINT('',#23541);
#7105=VERTEX_POINT('',#23545);
#7106=VERTEX_POINT('',#23547);
#7107=VERTEX_POINT('',#23551);
#7108=VERTEX_POINT('',#23553);
#7109=VERTEX_POINT('',#23557);
#7110=VERTEX_POINT('',#23559);
#7111=VERTEX_POINT('',#23563);
#7112=VERTEX_POINT('',#23565);
#7113=VERTEX_POINT('',#23569);
#7114=VERTEX_POINT('',#23570);
#7115=VERTEX_POINT('',#23572);
#7116=VERTEX_POINT('',#23574);
#7117=VERTEX_POINT('',#23578);
#7118=VERTEX_POINT('',#23579);
#7119=VERTEX_POINT('',#23581);
#7120=VERTEX_POINT('',#23583);
#7121=VERTEX_POINT('',#23587);
#7122=VERTEX_POINT('',#23589);
#7123=VERTEX_POINT('',#23593);
#7124=VERTEX_POINT('',#23596);
#7125=VERTEX_POINT('',#23598);
#7126=VERTEX_POINT('',#23601);
#7127=VERTEX_POINT('',#23603);
#7128=VERTEX_POINT('',#23606);
#7129=VERTEX_POINT('',#23610);
#7130=VERTEX_POINT('',#23614);
#7131=VERTEX_POINT('',#23616);
#7132=VERTEX_POINT('',#23622);
#7133=VERTEX_POINT('',#23632);
#7134=VERTEX_POINT('',#23634);
#7135=VERTEX_POINT('',#23638);
#7136=VERTEX_POINT('',#23640);
#7137=VERTEX_POINT('',#23647);
#7138=VERTEX_POINT('',#23649);
#7139=VERTEX_POINT('',#23653);
#7140=VERTEX_POINT('',#23655);
#7141=VERTEX_POINT('',#23662);
#7142=VERTEX_POINT('',#23664);
#7143=VERTEX_POINT('',#23668);
#7144=VERTEX_POINT('',#23670);
#7145=VERTEX_POINT('',#23674);
#7146=VERTEX_POINT('',#23676);
#7147=VERTEX_POINT('',#23680);
#7148=VERTEX_POINT('',#23682);
#7149=VERTEX_POINT('',#23686);
#7150=VERTEX_POINT('',#23688);
#7151=VERTEX_POINT('',#23692);
#7152=VERTEX_POINT('',#23694);
#7153=VERTEX_POINT('',#23701);
#7154=VERTEX_POINT('',#23703);
#7155=VERTEX_POINT('',#23706);
#7156=VERTEX_POINT('',#23711);
#7157=VERTEX_POINT('',#23717);
#7158=VERTEX_POINT('',#23719);
#7159=VERTEX_POINT('',#23722);
#7160=VERTEX_POINT('',#23727);
#7161=VERTEX_POINT('',#23733);
#7162=VERTEX_POINT('',#23735);
#7163=VERTEX_POINT('',#23738);
#7164=VERTEX_POINT('',#23743);
#7165=VERTEX_POINT('',#23749);
#7166=VERTEX_POINT('',#23751);
#7167=VERTEX_POINT('',#23754);
#7168=VERTEX_POINT('',#23759);
#7169=VERTEX_POINT('',#23765);
#7170=VERTEX_POINT('',#23767);
#7171=VERTEX_POINT('',#23771);
#7172=VERTEX_POINT('',#23773);
#7173=VERTEX_POINT('',#23777);
#7174=VERTEX_POINT('',#23779);
#7175=VERTEX_POINT('',#23783);
#7176=VERTEX_POINT('',#23785);
#7177=VERTEX_POINT('',#23789);
#7178=VERTEX_POINT('',#23791);
#7179=VERTEX_POINT('',#23795);
#7180=VERTEX_POINT('',#23797);
#7181=VERTEX_POINT('',#23804);
#7182=VERTEX_POINT('',#23806);
#7183=VERTEX_POINT('',#23809);
#7184=VERTEX_POINT('',#23814);
#7185=VERTEX_POINT('',#23820);
#7186=VERTEX_POINT('',#23822);
#7187=VERTEX_POINT('',#23825);
#7188=VERTEX_POINT('',#23830);
#7189=VERTEX_POINT('',#23836);
#7190=VERTEX_POINT('',#23838);
#7191=VERTEX_POINT('',#23841);
#7192=VERTEX_POINT('',#23846);
#7193=VERTEX_POINT('',#23852);
#7194=VERTEX_POINT('',#23854);
#7195=VERTEX_POINT('',#23857);
#7196=VERTEX_POINT('',#23862);
#7197=VERTEX_POINT('',#23868);
#7198=VERTEX_POINT('',#23870);
#7199=VERTEX_POINT('',#23874);
#7200=VERTEX_POINT('',#23876);
#7201=VERTEX_POINT('',#23880);
#7202=VERTEX_POINT('',#23882);
#7203=VERTEX_POINT('',#23886);
#7204=VERTEX_POINT('',#23888);
#7205=VERTEX_POINT('',#23892);
#7206=VERTEX_POINT('',#23894);
#7207=VERTEX_POINT('',#23898);
#7208=VERTEX_POINT('',#23899);
#7209=VERTEX_POINT('',#23901);
#7210=VERTEX_POINT('',#23903);
#7211=VERTEX_POINT('',#23907);
#7212=VERTEX_POINT('',#23908);
#7213=VERTEX_POINT('',#23910);
#7214=VERTEX_POINT('',#23912);
#7215=VERTEX_POINT('',#23916);
#7216=VERTEX_POINT('',#23918);
#7217=VERTEX_POINT('',#23922);
#7218=VERTEX_POINT('',#23925);
#7219=VERTEX_POINT('',#23927);
#7220=VERTEX_POINT('',#23930);
#7221=VERTEX_POINT('',#23932);
#7222=VERTEX_POINT('',#23935);
#7223=VERTEX_POINT('',#23939);
#7224=VERTEX_POINT('',#23943);
#7225=VERTEX_POINT('',#23945);
#7226=VERTEX_POINT('',#23951);
#7227=VERTEX_POINT('',#23961);
#7228=VERTEX_POINT('',#23963);
#7229=VERTEX_POINT('',#23967);
#7230=VERTEX_POINT('',#23969);
#7231=VERTEX_POINT('',#23976);
#7232=VERTEX_POINT('',#23978);
#7233=VERTEX_POINT('',#23982);
#7234=VERTEX_POINT('',#23984);
#7235=VERTEX_POINT('',#23991);
#7236=VERTEX_POINT('',#23993);
#7237=VERTEX_POINT('',#23997);
#7238=VERTEX_POINT('',#23999);
#7239=VERTEX_POINT('',#24003);
#7240=VERTEX_POINT('',#24005);
#7241=VERTEX_POINT('',#24009);
#7242=VERTEX_POINT('',#24011);
#7243=VERTEX_POINT('',#24015);
#7244=VERTEX_POINT('',#24017);
#7245=VERTEX_POINT('',#24021);
#7246=VERTEX_POINT('',#24023);
#7247=VERTEX_POINT('',#24030);
#7248=VERTEX_POINT('',#24032);
#7249=VERTEX_POINT('',#24035);
#7250=VERTEX_POINT('',#24040);
#7251=VERTEX_POINT('',#24046);
#7252=VERTEX_POINT('',#24048);
#7253=VERTEX_POINT('',#24051);
#7254=VERTEX_POINT('',#24056);
#7255=VERTEX_POINT('',#24062);
#7256=VERTEX_POINT('',#24064);
#7257=VERTEX_POINT('',#24067);
#7258=VERTEX_POINT('',#24072);
#7259=VERTEX_POINT('',#24078);
#7260=VERTEX_POINT('',#24080);
#7261=VERTEX_POINT('',#24083);
#7262=VERTEX_POINT('',#24088);
#7263=VERTEX_POINT('',#24094);
#7264=VERTEX_POINT('',#24096);
#7265=VERTEX_POINT('',#24100);
#7266=VERTEX_POINT('',#24102);
#7267=VERTEX_POINT('',#24106);
#7268=VERTEX_POINT('',#24108);
#7269=VERTEX_POINT('',#24112);
#7270=VERTEX_POINT('',#24114);
#7271=VERTEX_POINT('',#24118);
#7272=VERTEX_POINT('',#24120);
#7273=VERTEX_POINT('',#24124);
#7274=VERTEX_POINT('',#24126);
#7275=VERTEX_POINT('',#24133);
#7276=VERTEX_POINT('',#24135);
#7277=VERTEX_POINT('',#24138);
#7278=VERTEX_POINT('',#24143);
#7279=VERTEX_POINT('',#24149);
#7280=VERTEX_POINT('',#24151);
#7281=VERTEX_POINT('',#24154);
#7282=VERTEX_POINT('',#24159);
#7283=VERTEX_POINT('',#24165);
#7284=VERTEX_POINT('',#24167);
#7285=VERTEX_POINT('',#24170);
#7286=VERTEX_POINT('',#24175);
#7287=VERTEX_POINT('',#24181);
#7288=VERTEX_POINT('',#24183);
#7289=VERTEX_POINT('',#24186);
#7290=VERTEX_POINT('',#24191);
#7291=VERTEX_POINT('',#24198);
#7292=VERTEX_POINT('',#24199);
#7293=VERTEX_POINT('',#24202);
#7294=VERTEX_POINT('',#24204);
#7295=VERTEX_POINT('',#24208);
#7296=VERTEX_POINT('',#24212);
#7297=VERTEX_POINT('',#24214);
#7298=VERTEX_POINT('',#24218);
#7299=VERTEX_POINT('',#24223);
#7300=VERTEX_POINT('',#24227);
#7301=VERTEX_POINT('',#24233);
#7302=VERTEX_POINT('',#24234);
#7303=VERTEX_POINT('',#24237);
#7304=VERTEX_POINT('',#24239);
#7305=VERTEX_POINT('',#24243);
#7306=VERTEX_POINT('',#24247);
#7307=VERTEX_POINT('',#24249);
#7308=VERTEX_POINT('',#24252);
#7309=VERTEX_POINT('',#24256);
#7310=VERTEX_POINT('',#24260);
#7311=VERTEX_POINT('',#24268);
#7312=VERTEX_POINT('',#24269);
#7313=VERTEX_POINT('',#24272);
#7314=VERTEX_POINT('',#24273);
#7315=VERTEX_POINT('',#24276);
#7316=VERTEX_POINT('',#24277);
#7317=VERTEX_POINT('',#24280);
#7318=VERTEX_POINT('',#24281);
#7319=VERTEX_POINT('',#24284);
#7320=VERTEX_POINT('',#24285);
#7321=VERTEX_POINT('',#24288);
#7322=VERTEX_POINT('',#24289);
#7323=VERTEX_POINT('',#24292);
#7324=VERTEX_POINT('',#24293);
#7325=VERTEX_POINT('',#24297);
#7326=VERTEX_POINT('',#24298);
#7327=VERTEX_POINT('',#24305);
#7328=VERTEX_POINT('',#24307);
#7329=VERTEX_POINT('',#24316);
#7330=VERTEX_POINT('',#24318);
#7331=VERTEX_POINT('',#24322);
#7332=VERTEX_POINT('',#24331);
#7333=VERTEX_POINT('',#24343);
#7334=VERTEX_POINT('',#24344);
#7335=VERTEX_POINT('',#24346);
#7336=VERTEX_POINT('',#24353);
#7337=VERTEX_POINT('',#24362);
#7338=VERTEX_POINT('',#24364);
#7339=VERTEX_POINT('',#24368);
#7340=VERTEX_POINT('',#24377);
#7341=VERTEX_POINT('',#24389);
#7342=VERTEX_POINT('',#24390);
#7343=VERTEX_POINT('',#24397);
#7344=VERTEX_POINT('',#24399);
#7345=VERTEX_POINT('',#24408);
#7346=VERTEX_POINT('',#24410);
#7347=VERTEX_POINT('',#24419);
#7348=VERTEX_POINT('',#24423);
#7349=VERTEX_POINT('',#24435);
#7350=VERTEX_POINT('',#24436);
#7351=VERTEX_POINT('',#24438);
#7352=VERTEX_POINT('',#24445);
#7353=VERTEX_POINT('',#24454);
#7354=VERTEX_POINT('',#24456);
#7355=VERTEX_POINT('',#24465);
#7356=VERTEX_POINT('',#24469);
#7357=VERTEX_POINT('',#24481);
#7358=VERTEX_POINT('',#24482);
#7359=VERTEX_POINT('',#24489);
#7360=VERTEX_POINT('',#24491);
#7361=VERTEX_POINT('',#24500);
#7362=VERTEX_POINT('',#24501);
#7363=VERTEX_POINT('',#24511);
#7364=VERTEX_POINT('',#24515);
#7365=VERTEX_POINT('',#24527);
#7366=VERTEX_POINT('',#24528);
#7367=VERTEX_POINT('',#24535);
#7368=VERTEX_POINT('',#24537);
#7369=VERTEX_POINT('',#24546);
#7370=VERTEX_POINT('',#24547);
#7371=VERTEX_POINT('',#24557);
#7372=VERTEX_POINT('',#24561);
#7373=VERTEX_POINT('',#24573);
#7374=VERTEX_POINT('',#24574);
#7375=VERTEX_POINT('',#24581);
#7376=VERTEX_POINT('',#24583);
#7377=VERTEX_POINT('',#24592);
#7378=VERTEX_POINT('',#24594);
#7379=VERTEX_POINT('',#24598);
#7380=VERTEX_POINT('',#24607);
#7381=VERTEX_POINT('',#24620);
#7382=VERTEX_POINT('',#24622);
#7383=VERTEX_POINT('',#24625);
#7384=VERTEX_POINT('',#24629);
#7385=VERTEX_POINT('',#24634);
#7386=VERTEX_POINT('',#24636);
#7387=VERTEX_POINT('',#24639);
#7388=VERTEX_POINT('',#24643);
#7389=VERTEX_POINT('',#24728);
#7390=VERTEX_POINT('',#24730);
#7391=VERTEX_POINT('',#24733);
#7392=VERTEX_POINT('',#24735);
#7393=VERTEX_POINT('',#24740);
#7394=VERTEX_POINT('',#24744);
#7395=VERTEX_POINT('',#24747);
#7396=VERTEX_POINT('',#24749);
#7397=VERTEX_POINT('',#24754);
#7398=VERTEX_POINT('',#24758);
#7399=VERTEX_POINT('',#24765);
#7400=VERTEX_POINT('',#24767);
#7401=VERTEX_POINT('',#24771);
#7402=VERTEX_POINT('',#24773);
#7403=VERTEX_POINT('',#24780);
#7404=VERTEX_POINT('',#24782);
#7405=VERTEX_POINT('',#24786);
#7406=VERTEX_POINT('',#24788);
#7407=VERTEX_POINT('',#24795);
#7408=VERTEX_POINT('',#24797);
#7409=VERTEX_POINT('',#24801);
#7410=VERTEX_POINT('',#24803);
#7411=VERTEX_POINT('',#24810);
#7412=VERTEX_POINT('',#24812);
#7413=VERTEX_POINT('',#24816);
#7414=VERTEX_POINT('',#24818);
#7415=VERTEX_POINT('',#24825);
#7416=VERTEX_POINT('',#24827);
#7417=VERTEX_POINT('',#24832);
#7418=VERTEX_POINT('',#24834);
#7419=VERTEX_POINT('',#24838);
#7420=VERTEX_POINT('',#24840);
#7421=EDGE_CURVE('',#6383,#6383,#5604,.T.);
#7422=EDGE_CURVE('',#6383,#6384,#4124,.T.);
#7423=EDGE_CURVE('',#6384,#6384,#5605,.T.);
#7424=EDGE_CURVE('',#6385,#6385,#5606,.T.);
#7425=EDGE_CURVE('',#6385,#6386,#4125,.T.);
#7426=EDGE_CURVE('',#6386,#6386,#5607,.T.);
#7427=EDGE_CURVE('',#6387,#6387,#5608,.T.);
#7428=EDGE_CURVE('',#6387,#6388,#4126,.T.);
#7429=EDGE_CURVE('',#6388,#6388,#5609,.T.);
#7430=EDGE_CURVE('',#6389,#6389,#5610,.T.);
#7431=EDGE_CURVE('',#6389,#6390,#4127,.T.);
#7432=EDGE_CURVE('',#6390,#6390,#5611,.T.);
#7433=EDGE_CURVE('',#6391,#6391,#5612,.T.);
#7434=EDGE_CURVE('',#6391,#6392,#4128,.T.);
#7435=EDGE_CURVE('',#6392,#6392,#5613,.T.);
#7436=EDGE_CURVE('',#6393,#6393,#5614,.T.);
#7437=EDGE_CURVE('',#6393,#6394,#4129,.T.);
#7438=EDGE_CURVE('',#6394,#6394,#5615,.T.);
#7439=EDGE_CURVE('',#6395,#6395,#5616,.T.);
#7440=EDGE_CURVE('',#6395,#6396,#4130,.T.);
#7441=EDGE_CURVE('',#6396,#6396,#5617,.T.);
#7442=EDGE_CURVE('',#6397,#6397,#5618,.T.);
#7443=EDGE_CURVE('',#6397,#6398,#4131,.T.);
#7444=EDGE_CURVE('',#6398,#6398,#5619,.T.);
#7445=EDGE_CURVE('',#6399,#6400,#4132,.T.);
#7446=EDGE_CURVE('',#6400,#6401,#4133,.T.);
#7447=EDGE_CURVE('',#6402,#6401,#4134,.T.);
#7448=EDGE_CURVE('',#6399,#6402,#4135,.T.);
#7449=EDGE_CURVE('',#6403,#6399,#4136,.T.);
#7450=EDGE_CURVE('',#6404,#6402,#4137,.T.);
#7451=EDGE_CURVE('',#6403,#6404,#4138,.T.);
#7452=EDGE_CURVE('',#6405,#6403,#4139,.T.);
#7453=EDGE_CURVE('',#6406,#6404,#4140,.T.);
#7454=EDGE_CURVE('',#6405,#6406,#4141,.T.);
#7455=EDGE_CURVE('',#6400,#6405,#4142,.T.);
#7456=EDGE_CURVE('',#6401,#6406,#4143,.T.);
#7457=EDGE_CURVE('',#6407,#6408,#4144,.T.);
#7458=EDGE_CURVE('',#6408,#6409,#4145,.T.);
#7459=EDGE_CURVE('',#6410,#6409,#4146,.T.);
#7460=EDGE_CURVE('',#6407,#6410,#4147,.T.);
#7461=EDGE_CURVE('',#6411,#6407,#4148,.T.);
#7462=EDGE_CURVE('',#6412,#6410,#4149,.T.);
#7463=EDGE_CURVE('',#6411,#6412,#4150,.T.);
#7464=EDGE_CURVE('',#6413,#6411,#4151,.T.);
#7465=EDGE_CURVE('',#6414,#6412,#4152,.T.);
#7466=EDGE_CURVE('',#6413,#6414,#4153,.T.);
#7467=EDGE_CURVE('',#6408,#6413,#4154,.T.);
#7468=EDGE_CURVE('',#6409,#6414,#4155,.T.);
#7469=EDGE_CURVE('',#6415,#6416,#4156,.T.);
#7470=EDGE_CURVE('',#6416,#6417,#4157,.T.);
#7471=EDGE_CURVE('',#6418,#6417,#4158,.T.);
#7472=EDGE_CURVE('',#6415,#6418,#4159,.T.);
#7473=EDGE_CURVE('',#6419,#6415,#4160,.T.);
#7474=EDGE_CURVE('',#6420,#6418,#4161,.T.);
#7475=EDGE_CURVE('',#6419,#6420,#4162,.T.);
#7476=EDGE_CURVE('',#6421,#6419,#4163,.T.);
#7477=EDGE_CURVE('',#6422,#6420,#4164,.T.);
#7478=EDGE_CURVE('',#6421,#6422,#4165,.T.);
#7479=EDGE_CURVE('',#6416,#6421,#4166,.T.);
#7480=EDGE_CURVE('',#6417,#6422,#4167,.T.);
#7481=EDGE_CURVE('',#6423,#6423,#5620,.T.);
#7482=EDGE_CURVE('',#6423,#6424,#4168,.T.);
#7483=EDGE_CURVE('',#6424,#6424,#5621,.T.);
#7484=EDGE_CURVE('',#6425,#6425,#5622,.T.);
#7485=EDGE_CURVE('',#6425,#6426,#4169,.T.);
#7486=EDGE_CURVE('',#6426,#6426,#5623,.T.);
#7487=EDGE_CURVE('',#6427,#6427,#5624,.T.);
#7488=EDGE_CURVE('',#6427,#6428,#4170,.T.);
#7489=EDGE_CURVE('',#6428,#6428,#5625,.T.);
#7490=EDGE_CURVE('',#6429,#6429,#5626,.T.);
#7491=EDGE_CURVE('',#6429,#6430,#4171,.T.);
#7492=EDGE_CURVE('',#6430,#6430,#5627,.T.);
#7493=EDGE_CURVE('',#6431,#6431,#5628,.T.);
#7494=EDGE_CURVE('',#6431,#6432,#4172,.T.);
#7495=EDGE_CURVE('',#6432,#6432,#5629,.T.);
#7496=EDGE_CURVE('',#6433,#6433,#5630,.T.);
#7497=EDGE_CURVE('',#6433,#6434,#4173,.T.);
#7498=EDGE_CURVE('',#6434,#6434,#5631,.T.);
#7499=EDGE_CURVE('',#6435,#6435,#5632,.T.);
#7500=EDGE_CURVE('',#6435,#6436,#4174,.T.);
#7501=EDGE_CURVE('',#6436,#6436,#5633,.T.);
#7502=EDGE_CURVE('',#6437,#6437,#5634,.T.);
#7503=EDGE_CURVE('',#6437,#6438,#4175,.T.);
#7504=EDGE_CURVE('',#6438,#6438,#5635,.T.);
#7505=EDGE_CURVE('',#6439,#6439,#5636,.T.);
#7506=EDGE_CURVE('',#6439,#6440,#4176,.T.);
#7507=EDGE_CURVE('',#6440,#6440,#5637,.T.);
#7508=EDGE_CURVE('',#6441,#6442,#4177,.T.);
#7509=EDGE_CURVE('',#6441,#6443,#4178,.T.);
#7510=EDGE_CURVE('',#6443,#6444,#4179,.T.);
#7511=EDGE_CURVE('',#6444,#6442,#4180,.T.);
#7512=EDGE_CURVE('',#6445,#6446,#4181,.T.);
#7513=EDGE_CURVE('',#6445,#6447,#4182,.T.);
#7514=EDGE_CURVE('',#6447,#6448,#4183,.T.);
#7515=EDGE_CURVE('',#6448,#6446,#4184,.T.);
#7516=EDGE_CURVE('',#6449,#6450,#4185,.T.);
#7517=EDGE_CURVE('',#6450,#6448,#4186,.T.);
#7518=EDGE_CURVE('',#6449,#6447,#4187,.T.);
#7519=EDGE_CURVE('',#6451,#6452,#4188,.T.);
#7520=EDGE_CURVE('',#6452,#6444,#4189,.T.);
#7521=EDGE_CURVE('',#6451,#6443,#4190,.T.);
#7522=EDGE_CURVE('',#6441,#6453,#4191,.T.);
#7523=EDGE_CURVE('',#6454,#6453,#4192,.T.);
#7524=EDGE_CURVE('',#6446,#6454,#4193,.T.);
#7525=EDGE_CURVE('',#6450,#6451,#4194,.T.);
#7526=EDGE_CURVE('',#6455,#6455,#5638,.T.);
#7527=EDGE_CURVE('',#6442,#6456,#4195,.T.);
#7528=EDGE_CURVE('',#6453,#6456,#4196,.T.);
#7529=EDGE_CURVE('',#6457,#6457,#5639,.T.);
#7530=EDGE_CURVE('',#6458,#6458,#5640,.T.);
#7531=EDGE_CURVE('',#6459,#6459,#5641,.T.);
#7532=EDGE_CURVE('',#6459,#6455,#4197,.T.);
#7533=EDGE_CURVE('',#6457,#6460,#4198,.T.);
#7534=EDGE_CURVE('',#6460,#6460,#5642,.T.);
#7535=EDGE_CURVE('',#6458,#6461,#4199,.T.);
#7536=EDGE_CURVE('',#6461,#6461,#5643,.T.);
#7537=EDGE_CURVE('',#6462,#6454,#4200,.T.);
#7538=EDGE_CURVE('',#6445,#6462,#4201,.T.);
#7539=EDGE_CURVE('',#6456,#6462,#4202,.T.);
#7540=EDGE_CURVE('',#6452,#6449,#4203,.T.);
#7541=EDGE_CURVE('',#6463,#6463,#5644,.T.);
#7542=EDGE_CURVE('',#6463,#6464,#4204,.T.);
#7543=EDGE_CURVE('',#6464,#6464,#5645,.T.);
#7544=EDGE_CURVE('',#6465,#6465,#5646,.T.);
#7545=EDGE_CURVE('',#6465,#6466,#4205,.T.);
#7546=EDGE_CURVE('',#6466,#6466,#5647,.T.);
#7547=EDGE_CURVE('',#6467,#6467,#5648,.T.);
#7548=EDGE_CURVE('',#6467,#6468,#4206,.T.);
#7549=EDGE_CURVE('',#6468,#6468,#5649,.T.);
#7550=EDGE_CURVE('',#6469,#6469,#5650,.T.);
#7551=EDGE_CURVE('',#6469,#6470,#4207,.T.);
#7552=EDGE_CURVE('',#6470,#6470,#5651,.T.);
#7553=EDGE_CURVE('',#6471,#6471,#5652,.T.);
#7554=EDGE_CURVE('',#6471,#6472,#4208,.T.);
#7555=EDGE_CURVE('',#6472,#6472,#5653,.T.);
#7556=EDGE_CURVE('',#6473,#6473,#5654,.T.);
#7557=EDGE_CURVE('',#6473,#6474,#4209,.T.);
#7558=EDGE_CURVE('',#6474,#6474,#5655,.T.);
#7559=EDGE_CURVE('',#6475,#6475,#5656,.T.);
#7560=EDGE_CURVE('',#6475,#6476,#4210,.T.);
#7561=EDGE_CURVE('',#6476,#6476,#5657,.T.);
#7562=EDGE_CURVE('',#6477,#6477,#5658,.T.);
#7563=EDGE_CURVE('',#6477,#6478,#4211,.T.);
#7564=EDGE_CURVE('',#6478,#6478,#5659,.T.);
#7565=EDGE_CURVE('',#6479,#6479,#5660,.T.);
#7566=EDGE_CURVE('',#6479,#6480,#4212,.T.);
#7567=EDGE_CURVE('',#6480,#6480,#5661,.T.);
#7568=EDGE_CURVE('',#6481,#6481,#5662,.T.);
#7569=EDGE_CURVE('',#6481,#6482,#4213,.T.);
#7570=EDGE_CURVE('',#6482,#6482,#5663,.T.);
#7571=EDGE_CURVE('',#6483,#6483,#5664,.T.);
#7572=EDGE_CURVE('',#6483,#6484,#4214,.T.);
#7573=EDGE_CURVE('',#6484,#6484,#5665,.T.);
#7574=EDGE_CURVE('',#6485,#6485,#5666,.T.);
#7575=EDGE_CURVE('',#6485,#6486,#4215,.T.);
#7576=EDGE_CURVE('',#6486,#6486,#5667,.T.);
#7577=EDGE_CURVE('',#6487,#6487,#5668,.T.);
#7578=EDGE_CURVE('',#6488,#6488,#5669,.T.);
#7579=EDGE_CURVE('',#6488,#6487,#4216,.T.);
#7580=EDGE_CURVE('',#6489,#6489,#5670,.T.);
#7581=EDGE_CURVE('',#6489,#6490,#4217,.T.);
#7582=EDGE_CURVE('',#6490,#6490,#5671,.T.);
#7583=EDGE_CURVE('',#6491,#6491,#5672,.T.);
#7584=EDGE_CURVE('',#6491,#6492,#4218,.T.);
#7585=EDGE_CURVE('',#6492,#6492,#5673,.T.);
#7586=EDGE_CURVE('',#6493,#6493,#5674,.T.);
#7587=EDGE_CURVE('',#6493,#6494,#4219,.T.);
#7588=EDGE_CURVE('',#6494,#6494,#5675,.T.);
#7589=EDGE_CURVE('',#6495,#6495,#5676,.T.);
#7590=EDGE_CURVE('',#6495,#6496,#4220,.T.);
#7591=EDGE_CURVE('',#6496,#6496,#5677,.T.);
#7592=EDGE_CURVE('',#6497,#6497,#5678,.T.);
#7593=EDGE_CURVE('',#6497,#6498,#4221,.T.);
#7594=EDGE_CURVE('',#6498,#6498,#5679,.T.);
#7595=EDGE_CURVE('',#6499,#6499,#5680,.T.);
#7596=EDGE_CURVE('',#6499,#6500,#4222,.T.);
#7597=EDGE_CURVE('',#6500,#6500,#5681,.T.);
#7598=EDGE_CURVE('',#6501,#6501,#5682,.T.);
#7599=EDGE_CURVE('',#6501,#6502,#4223,.T.);
#7600=EDGE_CURVE('',#6502,#6502,#5683,.T.);
#7601=EDGE_CURVE('',#6503,#6503,#5684,.T.);
#7602=EDGE_CURVE('',#6503,#6504,#4224,.T.);
#7603=EDGE_CURVE('',#6504,#6504,#5685,.T.);
#7604=EDGE_CURVE('',#6505,#6505,#5686,.T.);
#7605=EDGE_CURVE('',#6505,#6506,#4225,.T.);
#7606=EDGE_CURVE('',#6506,#6506,#5687,.T.);
#7607=EDGE_CURVE('',#6507,#6507,#5688,.T.);
#7608=EDGE_CURVE('',#6507,#6508,#4226,.T.);
#7609=EDGE_CURVE('',#6508,#6508,#5689,.T.);
#7610=EDGE_CURVE('',#6509,#6510,#4227,.T.);
#7611=EDGE_CURVE('',#6509,#6511,#4228,.T.);
#7612=EDGE_CURVE('',#6511,#6512,#4229,.T.);
#7613=EDGE_CURVE('',#6512,#6510,#4230,.T.);
#7614=EDGE_CURVE('',#6513,#6514,#4231,.T.);
#7615=EDGE_CURVE('',#6513,#6515,#4232,.T.);
#7616=EDGE_CURVE('',#6515,#6516,#4233,.T.);
#7617=EDGE_CURVE('',#6516,#6514,#4234,.T.);
#7618=EDGE_CURVE('',#6517,#6518,#4235,.T.);
#7619=EDGE_CURVE('',#6518,#6516,#4236,.T.);
#7620=EDGE_CURVE('',#6517,#6515,#4237,.T.);
#7621=EDGE_CURVE('',#6519,#6520,#4238,.T.);
#7622=EDGE_CURVE('',#6520,#6512,#4239,.T.);
#7623=EDGE_CURVE('',#6519,#6511,#4240,.T.);
#7624=EDGE_CURVE('',#6509,#6521,#4241,.T.);
#7625=EDGE_CURVE('',#6522,#6521,#4242,.T.);
#7626=EDGE_CURVE('',#6514,#6522,#4243,.T.);
#7627=EDGE_CURVE('',#6518,#6519,#4244,.T.);
#7628=EDGE_CURVE('',#6510,#6523,#4245,.T.);
#7629=EDGE_CURVE('',#6521,#6523,#4246,.T.);
#7630=EDGE_CURVE('',#6524,#6524,#5690,.T.);
#7631=EDGE_CURVE('',#6525,#6525,#5691,.T.);
#7632=EDGE_CURVE('',#6524,#6526,#4247,.T.);
#7633=EDGE_CURVE('',#6526,#6526,#5692,.T.);
#7634=EDGE_CURVE('',#6525,#6527,#4248,.T.);
#7635=EDGE_CURVE('',#6527,#6527,#5693,.T.);
#7636=EDGE_CURVE('',#6528,#6522,#4249,.T.);
#7637=EDGE_CURVE('',#6513,#6528,#4250,.T.);
#7638=EDGE_CURVE('',#6523,#6528,#4251,.T.);
#7639=EDGE_CURVE('',#6520,#6517,#4252,.T.);
#7640=EDGE_CURVE('',#6529,#6529,#5694,.T.);
#7641=EDGE_CURVE('',#6529,#6530,#4253,.T.);
#7642=EDGE_CURVE('',#6530,#6530,#5695,.T.);
#7643=EDGE_CURVE('',#6531,#6531,#5696,.T.);
#7644=EDGE_CURVE('',#6531,#6532,#4254,.T.);
#7645=EDGE_CURVE('',#6532,#6532,#5697,.T.);
#7646=EDGE_CURVE('',#6533,#6533,#5698,.T.);
#7647=EDGE_CURVE('',#6533,#6534,#4255,.T.);
#7648=EDGE_CURVE('',#6534,#6534,#5699,.T.);
#7649=EDGE_CURVE('',#6535,#6535,#5700,.T.);
#7650=EDGE_CURVE('',#6535,#6536,#4256,.T.);
#7651=EDGE_CURVE('',#6536,#6536,#5701,.T.);
#7652=EDGE_CURVE('',#6537,#6537,#5702,.T.);
#7653=EDGE_CURVE('',#6537,#6538,#4257,.T.);
#7654=EDGE_CURVE('',#6538,#6538,#5703,.T.);
#7655=EDGE_CURVE('',#6539,#6539,#5704,.T.);
#7656=EDGE_CURVE('',#6539,#6540,#4258,.T.);
#7657=EDGE_CURVE('',#6540,#6540,#5705,.T.);
#7658=EDGE_CURVE('',#6541,#6541,#5706,.T.);
#7659=EDGE_CURVE('',#6541,#6542,#4259,.T.);
#7660=EDGE_CURVE('',#6542,#6542,#5707,.T.);
#7661=EDGE_CURVE('',#6543,#6543,#5708,.T.);
#7662=EDGE_CURVE('',#6543,#6544,#4260,.T.);
#7663=EDGE_CURVE('',#6544,#6544,#5709,.T.);
#7664=EDGE_CURVE('',#6545,#6545,#5710,.T.);
#7665=EDGE_CURVE('',#6545,#6546,#4261,.T.);
#7666=EDGE_CURVE('',#6546,#6546,#5711,.T.);
#7667=EDGE_CURVE('',#6547,#6547,#5712,.T.);
#7668=EDGE_CURVE('',#6547,#6548,#4262,.T.);
#7669=EDGE_CURVE('',#6548,#6548,#5713,.T.);
#7670=EDGE_CURVE('',#6549,#6549,#5714,.T.);
#7671=EDGE_CURVE('',#6549,#6550,#4263,.T.);
#7672=EDGE_CURVE('',#6550,#6550,#5715,.T.);
#7673=EDGE_CURVE('',#6551,#6551,#5716,.T.);
#7674=EDGE_CURVE('',#6551,#6552,#4264,.T.);
#7675=EDGE_CURVE('',#6552,#6552,#5717,.T.);
#7676=EDGE_CURVE('',#6553,#6553,#5718,.T.);
#7677=EDGE_CURVE('',#6554,#6554,#5719,.T.);
#7678=EDGE_CURVE('',#6554,#6553,#4265,.T.);
#7679=EDGE_CURVE('',#6555,#6555,#5720,.T.);
#7680=EDGE_CURVE('',#6555,#6556,#4266,.T.);
#7681=EDGE_CURVE('',#6556,#6556,#5721,.T.);
#7682=EDGE_CURVE('',#6557,#6557,#5722,.T.);
#7683=EDGE_CURVE('',#6557,#6558,#4267,.T.);
#7684=EDGE_CURVE('',#6558,#6558,#5723,.T.);
#7685=EDGE_CURVE('',#6559,#6559,#5724,.T.);
#7686=EDGE_CURVE('',#6559,#6560,#4268,.T.);
#7687=EDGE_CURVE('',#6560,#6560,#5725,.T.);
#7688=EDGE_CURVE('',#6561,#6561,#5726,.T.);
#7689=EDGE_CURVE('',#6561,#6562,#4269,.T.);
#7690=EDGE_CURVE('',#6562,#6562,#5727,.T.);
#7691=EDGE_CURVE('',#6563,#6563,#5728,.T.);
#7692=EDGE_CURVE('',#6563,#6564,#4270,.T.);
#7693=EDGE_CURVE('',#6564,#6564,#5729,.T.);
#7694=EDGE_CURVE('',#6565,#6565,#5730,.T.);
#7695=EDGE_CURVE('',#6565,#6566,#4271,.T.);
#7696=EDGE_CURVE('',#6566,#6566,#5731,.T.);
#7697=EDGE_CURVE('',#6567,#6567,#5732,.T.);
#7698=EDGE_CURVE('',#6567,#6568,#4272,.T.);
#7699=EDGE_CURVE('',#6568,#6568,#5733,.T.);
#7700=EDGE_CURVE('',#6569,#6569,#5734,.T.);
#7701=EDGE_CURVE('',#6569,#6570,#4273,.T.);
#7702=EDGE_CURVE('',#6570,#6570,#5735,.T.);
#7703=EDGE_CURVE('',#6571,#6571,#5736,.T.);
#7704=EDGE_CURVE('',#6571,#6572,#4274,.T.);
#7705=EDGE_CURVE('',#6572,#6572,#5737,.T.);
#7706=EDGE_CURVE('',#6573,#6573,#5738,.T.);
#7707=EDGE_CURVE('',#6573,#6574,#4275,.T.);
#7708=EDGE_CURVE('',#6574,#6574,#5739,.T.);
#7709=EDGE_CURVE('',#6575,#6575,#5740,.T.);
#7710=EDGE_CURVE('',#6575,#6576,#4276,.T.);
#7711=EDGE_CURVE('',#6576,#6576,#5741,.T.);
#7712=EDGE_CURVE('',#6577,#6577,#5742,.T.);
#7713=EDGE_CURVE('',#6577,#6578,#4277,.T.);
#7714=EDGE_CURVE('',#6578,#6578,#5743,.T.);
#7715=EDGE_CURVE('',#6579,#6579,#5744,.T.);
#7716=EDGE_CURVE('',#6579,#6580,#4278,.T.);
#7717=EDGE_CURVE('',#6580,#6580,#5745,.T.);
#7718=EDGE_CURVE('',#6581,#6581,#5746,.T.);
#7719=EDGE_CURVE('',#6581,#6582,#4279,.T.);
#7720=EDGE_CURVE('',#6582,#6582,#5747,.T.);
#7721=EDGE_CURVE('',#6583,#6583,#5748,.T.);
#7722=EDGE_CURVE('',#6583,#6584,#4280,.T.);
#7723=EDGE_CURVE('',#6584,#6584,#5749,.T.);
#7724=EDGE_CURVE('',#6585,#6585,#5750,.T.);
#7725=EDGE_CURVE('',#6585,#6586,#4281,.T.);
#7726=EDGE_CURVE('',#6586,#6586,#5751,.T.);
#7727=EDGE_CURVE('',#6587,#6588,#4282,.T.);
#7728=EDGE_CURVE('',#6588,#6589,#4283,.T.);
#7729=EDGE_CURVE('',#6589,#6590,#4284,.T.);
#7730=EDGE_CURVE('',#6587,#6590,#4285,.T.);
#7731=EDGE_CURVE('',#6588,#6591,#4286,.T.);
#7732=EDGE_CURVE('',#6591,#6592,#4287,.T.);
#7733=EDGE_CURVE('',#6592,#6589,#4288,.T.);
#7734=EDGE_CURVE('',#6591,#6593,#4289,.T.);
#7735=EDGE_CURVE('',#6593,#6594,#4290,.T.);
#7736=EDGE_CURVE('',#6594,#6592,#4291,.T.);
#7737=EDGE_CURVE('',#6593,#6595,#4292,.T.);
#7738=EDGE_CURVE('',#6595,#6596,#4293,.T.);
#7739=EDGE_CURVE('',#6596,#6594,#4294,.T.);
#7740=EDGE_CURVE('',#6595,#6597,#4295,.T.);
#7741=EDGE_CURVE('',#6597,#6598,#4296,.T.);
#7742=EDGE_CURVE('',#6598,#6596,#4297,.T.);
#7743=EDGE_CURVE('',#6597,#6587,#4298,.T.);
#7744=EDGE_CURVE('',#6590,#6598,#4299,.T.);
#7745=EDGE_CURVE('',#6599,#6599,#5752,.T.);
#7746=EDGE_CURVE('',#6600,#6600,#5753,.T.);
#7747=EDGE_CURVE('',#6601,#6601,#5754,.T.);
#7748=EDGE_CURVE('',#6601,#6600,#4300,.T.);
#7749=EDGE_CURVE('',#6602,#6602,#5755,.T.);
#7750=EDGE_CURVE('',#6602,#6601,#4301,.T.);
#7751=EDGE_CURVE('',#6603,#6603,#5756,.T.);
#7752=EDGE_CURVE('',#6603,#6602,#4302,.T.);
#7753=EDGE_CURVE('',#6604,#6604,#5757,.T.);
#7754=EDGE_CURVE('',#6605,#6605,#5758,.F.);
#7755=EDGE_CURVE('',#6605,#6604,#4303,.T.);
#7756=EDGE_CURVE('',#6599,#6605,#4304,.T.);
#7757=EDGE_CURVE('',#6606,#6606,#5759,.T.);
#7758=EDGE_CURVE('',#6606,#6607,#4305,.T.);
#7759=EDGE_CURVE('',#6607,#6607,#5760,.T.);
#7760=EDGE_CURVE('',#6608,#6608,#5761,.T.);
#7761=EDGE_CURVE('',#6608,#6609,#4306,.T.);
#7762=EDGE_CURVE('',#6609,#6609,#5762,.T.);
#7763=EDGE_CURVE('',#6610,#6610,#5763,.T.);
#7764=EDGE_CURVE('',#6610,#6611,#4307,.T.);
#7765=EDGE_CURVE('',#6611,#6611,#5764,.T.);
#7766=EDGE_CURVE('',#6612,#6612,#5765,.T.);
#7767=EDGE_CURVE('',#6612,#6613,#4308,.T.);
#7768=EDGE_CURVE('',#6613,#6613,#5766,.T.);
#7769=EDGE_CURVE('',#6614,#6614,#5767,.T.);
#7770=EDGE_CURVE('',#6614,#6615,#4309,.T.);
#7771=EDGE_CURVE('',#6615,#6615,#5768,.T.);
#7772=EDGE_CURVE('',#6616,#6616,#5769,.T.);
#7773=EDGE_CURVE('',#6616,#6617,#4310,.T.);
#7774=EDGE_CURVE('',#6617,#6617,#5770,.T.);
#7775=EDGE_CURVE('',#6618,#6618,#5771,.T.);
#7776=EDGE_CURVE('',#6618,#6619,#4311,.T.);
#7777=EDGE_CURVE('',#6619,#6619,#5772,.T.);
#7778=EDGE_CURVE('',#6620,#6620,#5773,.T.);
#7779=EDGE_CURVE('',#6620,#6621,#4312,.T.);
#7780=EDGE_CURVE('',#6621,#6621,#5774,.T.);
#7781=EDGE_CURVE('',#6622,#6623,#4313,.T.);
#7782=EDGE_CURVE('',#6623,#6624,#4314,.T.);
#7783=EDGE_CURVE('',#6625,#6624,#4315,.T.);
#7784=EDGE_CURVE('',#6622,#6625,#4316,.T.);
#7785=EDGE_CURVE('',#6626,#6622,#4317,.T.);
#7786=EDGE_CURVE('',#6627,#6625,#4318,.T.);
#7787=EDGE_CURVE('',#6626,#6627,#4319,.T.);
#7788=EDGE_CURVE('',#6628,#6626,#4320,.T.);
#7789=EDGE_CURVE('',#6629,#6627,#4321,.T.);
#7790=EDGE_CURVE('',#6628,#6629,#4322,.T.);
#7791=EDGE_CURVE('',#6623,#6628,#4323,.T.);
#7792=EDGE_CURVE('',#6624,#6629,#4324,.T.);
#7793=EDGE_CURVE('',#6630,#6630,#5775,.T.);
#7794=EDGE_CURVE('',#6630,#6631,#4325,.T.);
#7795=EDGE_CURVE('',#6631,#6631,#5776,.T.);
#7796=EDGE_CURVE('',#6632,#6632,#5777,.T.);
#7797=EDGE_CURVE('',#6632,#6633,#4326,.T.);
#7798=EDGE_CURVE('',#6633,#6633,#5778,.T.);
#7799=EDGE_CURVE('',#6634,#6634,#5779,.T.);
#7800=EDGE_CURVE('',#6634,#6635,#4327,.T.);
#7801=EDGE_CURVE('',#6635,#6635,#5780,.T.);
#7802=EDGE_CURVE('',#6636,#6636,#5781,.T.);
#7803=EDGE_CURVE('',#6636,#6637,#4328,.T.);
#7804=EDGE_CURVE('',#6637,#6637,#5782,.T.);
#7805=EDGE_CURVE('',#6638,#6639,#4329,.T.);
#7806=EDGE_CURVE('',#6640,#6638,#4330,.T.);
#7807=EDGE_CURVE('',#6641,#6640,#4331,.T.);
#7808=EDGE_CURVE('',#6639,#6641,#4332,.T.);
#7809=EDGE_CURVE('',#6642,#6643,#4333,.T.);
#7810=EDGE_CURVE('',#6644,#6642,#4334,.T.);
#7811=EDGE_CURVE('',#6645,#6644,#4335,.T.);
#7812=EDGE_CURVE('',#6643,#6645,#4336,.T.);
#7813=EDGE_CURVE('',#6638,#6646,#4337,.T.);
#7814=EDGE_CURVE('',#6647,#6646,#4338,.T.);
#7815=EDGE_CURVE('',#6640,#6647,#4339,.T.);
#7816=EDGE_CURVE('',#6648,#6647,#4340,.T.);
#7817=EDGE_CURVE('',#6641,#6648,#4341,.T.);
#7818=EDGE_CURVE('',#6649,#6648,#4342,.T.);
#7819=EDGE_CURVE('',#6639,#6649,#4343,.T.);
#7820=EDGE_CURVE('',#6646,#6649,#4344,.T.);
#7821=EDGE_CURVE('',#6650,#6644,#4345,.T.);
#7822=EDGE_CURVE('',#6650,#6651,#4346,.T.);
#7823=EDGE_CURVE('',#6651,#6645,#4347,.T.);
#7824=EDGE_CURVE('',#6652,#6652,#5783,.T.);
#7825=EDGE_CURVE('',#6653,#6642,#4348,.T.);
#7826=EDGE_CURVE('',#6653,#6650,#4349,.T.);
#7827=EDGE_CURVE('',#6654,#6654,#5784,.T.);
#7828=EDGE_CURVE('',#6655,#6655,#5785,.T.);
#7829=EDGE_CURVE('',#6652,#6656,#4350,.T.);
#7830=EDGE_CURVE('',#6656,#6656,#5786,.T.);
#7831=EDGE_CURVE('',#6655,#6657,#4351,.T.);
#7832=EDGE_CURVE('',#6657,#6657,#5787,.T.);
#7833=EDGE_CURVE('',#6654,#6658,#4352,.T.);
#7834=EDGE_CURVE('',#6658,#6658,#5788,.T.);
#7835=EDGE_CURVE('',#6659,#6643,#4353,.T.);
#7836=EDGE_CURVE('',#6659,#6653,#4354,.T.);
#7837=EDGE_CURVE('',#6651,#6659,#4355,.T.);
#7838=EDGE_CURVE('',#6660,#6660,#5789,.T.);
#7839=EDGE_CURVE('',#6660,#6661,#4356,.T.);
#7840=EDGE_CURVE('',#6661,#6661,#5790,.T.);
#7841=EDGE_CURVE('',#6662,#6662,#5791,.T.);
#7842=EDGE_CURVE('',#6662,#6663,#4357,.T.);
#7843=EDGE_CURVE('',#6663,#6663,#5792,.T.);
#7844=EDGE_CURVE('',#6664,#6664,#5793,.T.);
#7845=EDGE_CURVE('',#6664,#6665,#4358,.T.);
#7846=EDGE_CURVE('',#6665,#6665,#5794,.T.);
#7847=EDGE_CURVE('',#6666,#6666,#5795,.T.);
#7848=EDGE_CURVE('',#6666,#6667,#4359,.T.);
#7849=EDGE_CURVE('',#6667,#6667,#5796,.T.);
#7850=EDGE_CURVE('',#6668,#6669,#4360,.T.);
#7851=EDGE_CURVE('',#6670,#6668,#4361,.T.);
#7852=EDGE_CURVE('',#6671,#6670,#4362,.T.);
#7853=EDGE_CURVE('',#6669,#6671,#4363,.T.);
#7854=EDGE_CURVE('',#6672,#6673,#4364,.T.);
#7855=EDGE_CURVE('',#6673,#6674,#4365,.T.);
#7856=EDGE_CURVE('',#6675,#6674,#4366,.T.);
#7857=EDGE_CURVE('',#6672,#6675,#4367,.T.);
#7858=EDGE_CURVE('',#6670,#6676,#4368,.T.);
#7859=EDGE_CURVE('',#6677,#6676,#4369,.T.);
#7860=EDGE_CURVE('',#6671,#6677,#4370,.T.);
#7861=EDGE_CURVE('',#6678,#6679,#4371,.T.);
#7862=EDGE_CURVE('',#6673,#6678,#4372,.T.);
#7863=EDGE_CURVE('',#6679,#6672,#4373,.T.);
#7864=EDGE_CURVE('',#6680,#6679,#4374,.T.);
#7865=EDGE_CURVE('',#6680,#6681,#4375,.T.);
#7866=EDGE_CURVE('',#6681,#6678,#4376,.T.);
#7867=EDGE_CURVE('',#6682,#6682,#5797,.T.);
#7868=EDGE_CURVE('',#6683,#6683,#5798,.T.);
#7869=EDGE_CURVE('',#6684,#6668,#4377,.T.);
#7870=EDGE_CURVE('',#6684,#6680,#4378,.T.);
#7871=EDGE_CURVE('',#6676,#6675,#4379,.T.);
#7872=EDGE_CURVE('',#6685,#6685,#5799,.T.);
#7873=EDGE_CURVE('',#6685,#6683,#4380,.T.);
#7874=EDGE_CURVE('',#6686,#6686,#5800,.T.);
#7875=EDGE_CURVE('',#6686,#6682,#4381,.T.);
#7876=EDGE_CURVE('',#6681,#6687,#4382,.T.);
#7877=EDGE_CURVE('',#6687,#6669,#4383,.T.);
#7878=EDGE_CURVE('',#6674,#6677,#4384,.T.);
#7879=EDGE_CURVE('',#6687,#6684,#4385,.T.);
#7880=EDGE_CURVE('',#6688,#6688,#5801,.T.);
#7881=EDGE_CURVE('',#6688,#6689,#4386,.T.);
#7882=EDGE_CURVE('',#6689,#6689,#5802,.T.);
#7883=EDGE_CURVE('',#6690,#6690,#5803,.T.);
#7884=EDGE_CURVE('',#6690,#6691,#4387,.T.);
#7885=EDGE_CURVE('',#6691,#6691,#5804,.T.);
#7886=EDGE_CURVE('',#6692,#6692,#5805,.T.);
#7887=EDGE_CURVE('',#6692,#6693,#4388,.T.);
#7888=EDGE_CURVE('',#6693,#6693,#5806,.T.);
#7889=EDGE_CURVE('',#6694,#6694,#5807,.T.);
#7890=EDGE_CURVE('',#6694,#6695,#4389,.T.);
#7891=EDGE_CURVE('',#6695,#6695,#5808,.T.);
#7892=EDGE_CURVE('',#6696,#6696,#5809,.T.);
#7893=EDGE_CURVE('',#6696,#6697,#4390,.T.);
#7894=EDGE_CURVE('',#6697,#6697,#5810,.T.);
#7895=EDGE_CURVE('',#6698,#6698,#5811,.T.);
#7896=EDGE_CURVE('',#6698,#6699,#4391,.T.);
#7897=EDGE_CURVE('',#6699,#6699,#5812,.T.);
#7898=EDGE_CURVE('',#6700,#6700,#5813,.T.);
#7899=EDGE_CURVE('',#6700,#6701,#4392,.T.);
#7900=EDGE_CURVE('',#6701,#6701,#5814,.T.);
#7901=EDGE_CURVE('',#6702,#6702,#5815,.T.);
#7902=EDGE_CURVE('',#6702,#6703,#4393,.T.);
#7903=EDGE_CURVE('',#6703,#6703,#5816,.T.);
#7904=EDGE_CURVE('',#6704,#6704,#5817,.T.);
#7905=EDGE_CURVE('',#6704,#6705,#4394,.T.);
#7906=EDGE_CURVE('',#6705,#6705,#5818,.T.);
#7907=EDGE_CURVE('',#6706,#6706,#5819,.T.);
#7908=EDGE_CURVE('',#6706,#6707,#4395,.T.);
#7909=EDGE_CURVE('',#6707,#6707,#5820,.T.);
#7910=EDGE_CURVE('',#6708,#6708,#5821,.T.);
#7911=EDGE_CURVE('',#6708,#6709,#4396,.T.);
#7912=EDGE_CURVE('',#6709,#6709,#5822,.T.);
#7913=EDGE_CURVE('',#6710,#6710,#5823,.T.);
#7914=EDGE_CURVE('',#6710,#6711,#4397,.T.);
#7915=EDGE_CURVE('',#6711,#6711,#5824,.T.);
#7916=EDGE_CURVE('',#6712,#6712,#5825,.T.);
#7917=EDGE_CURVE('',#6712,#6713,#4398,.T.);
#7918=EDGE_CURVE('',#6713,#6713,#5826,.T.);
#7919=EDGE_CURVE('',#6714,#6714,#5827,.T.);
#7920=EDGE_CURVE('',#6714,#6715,#4399,.T.);
#7921=EDGE_CURVE('',#6715,#6715,#5828,.T.);
#7922=EDGE_CURVE('',#6716,#6716,#5829,.T.);
#7923=EDGE_CURVE('',#6716,#6717,#4400,.T.);
#7924=EDGE_CURVE('',#6717,#6717,#5830,.T.);
#7925=EDGE_CURVE('',#6718,#6718,#5831,.T.);
#7926=EDGE_CURVE('',#6718,#6719,#4401,.T.);
#7927=EDGE_CURVE('',#6719,#6719,#5832,.T.);
#7928=EDGE_CURVE('',#6720,#6720,#5833,.T.);
#7929=EDGE_CURVE('',#6720,#6721,#4402,.T.);
#7930=EDGE_CURVE('',#6721,#6721,#5834,.T.);
#7931=EDGE_CURVE('',#6722,#6722,#5835,.T.);
#7932=EDGE_CURVE('',#6723,#6723,#5836,.T.);
#7933=EDGE_CURVE('',#6723,#6722,#4403,.T.);
#7934=EDGE_CURVE('',#6724,#6724,#5837,.T.);
#7935=EDGE_CURVE('',#6724,#6723,#4404,.T.);
#7936=EDGE_CURVE('',#6725,#6725,#5838,.T.);
#7937=EDGE_CURVE('',#6725,#6724,#4405,.T.);
#7938=EDGE_CURVE('',#6726,#6726,#5839,.T.);
#7939=EDGE_CURVE('',#6727,#6727,#5840,.F.);
#7940=EDGE_CURVE('',#6727,#6726,#4406,.T.);
#7941=EDGE_CURVE('',#6728,#6728,#5841,.F.);
#7942=EDGE_CURVE('',#6728,#6727,#4407,.T.);
#7943=EDGE_CURVE('',#6729,#6729,#5842,.T.);
#7944=EDGE_CURVE('',#6729,#6728,#4408,.T.);
#7945=EDGE_CURVE('',#6730,#6731,#4409,.T.);
#7946=EDGE_CURVE('',#6731,#6732,#4410,.T.);
#7947=EDGE_CURVE('',#6732,#6733,#4411,.T.);
#7948=EDGE_CURVE('',#6730,#6733,#4412,.T.);
#7949=EDGE_CURVE('',#6731,#6734,#4413,.T.);
#7950=EDGE_CURVE('',#6734,#6735,#4414,.T.);
#7951=EDGE_CURVE('',#6735,#6732,#4415,.T.);
#7952=EDGE_CURVE('',#6734,#6736,#4416,.T.);
#7953=EDGE_CURVE('',#6736,#6737,#4417,.T.);
#7954=EDGE_CURVE('',#6737,#6735,#4418,.T.);
#7955=EDGE_CURVE('',#6736,#6738,#4419,.T.);
#7956=EDGE_CURVE('',#6738,#6739,#4420,.T.);
#7957=EDGE_CURVE('',#6739,#6737,#4421,.T.);
#7958=EDGE_CURVE('',#6738,#6740,#4422,.T.);
#7959=EDGE_CURVE('',#6740,#6741,#4423,.T.);
#7960=EDGE_CURVE('',#6741,#6739,#4424,.T.);
#7961=EDGE_CURVE('',#6740,#6730,#4425,.T.);
#7962=EDGE_CURVE('',#6733,#6741,#4426,.T.);
#7963=EDGE_CURVE('',#6742,#6742,#5843,.T.);
#7964=EDGE_CURVE('',#6742,#6743,#4427,.T.);
#7965=EDGE_CURVE('',#6743,#6743,#5844,.T.);
#7966=EDGE_CURVE('',#6744,#6744,#5845,.T.);
#7967=EDGE_CURVE('',#6744,#6745,#4428,.T.);
#7968=EDGE_CURVE('',#6745,#6745,#5846,.T.);
#7969=EDGE_CURVE('',#6746,#6746,#5847,.T.);
#7970=EDGE_CURVE('',#6746,#6747,#4429,.T.);
#7971=EDGE_CURVE('',#6747,#6747,#5848,.T.);
#7972=EDGE_CURVE('',#6748,#6749,#4430,.T.);
#7973=EDGE_CURVE('',#6749,#6750,#4431,.T.);
#7974=EDGE_CURVE('',#6751,#6750,#4432,.T.);
#7975=EDGE_CURVE('',#6748,#6751,#4433,.T.);
#7976=EDGE_CURVE('',#6752,#6748,#4434,.T.);
#7977=EDGE_CURVE('',#6753,#6751,#4435,.T.);
#7978=EDGE_CURVE('',#6752,#6753,#4436,.T.);
#7979=EDGE_CURVE('',#6754,#6752,#4437,.T.);
#7980=EDGE_CURVE('',#6755,#6753,#4438,.T.);
#7981=EDGE_CURVE('',#6754,#6755,#4439,.T.);
#7982=EDGE_CURVE('',#6749,#6754,#4440,.T.);
#7983=EDGE_CURVE('',#6750,#6755,#4441,.T.);
#7984=EDGE_CURVE('',#6756,#6756,#5849,.T.);
#7985=EDGE_CURVE('',#6756,#6757,#4442,.T.);
#7986=EDGE_CURVE('',#6757,#6757,#5850,.T.);
#7987=EDGE_CURVE('',#6758,#6758,#5851,.T.);
#7988=EDGE_CURVE('',#6759,#6759,#5852,.T.);
#7989=EDGE_CURVE('',#6759,#6760,#4443,.T.);
#7990=EDGE_CURVE('',#6760,#6760,#5853,.T.);
#7991=EDGE_CURVE('',#6761,#6761,#5854,.T.);
#7992=EDGE_CURVE('',#6762,#6762,#5855,.T.);
#7993=EDGE_CURVE('',#6762,#6763,#4444,.T.);
#7994=EDGE_CURVE('',#6763,#6763,#5856,.T.);
#7995=EDGE_CURVE('',#6764,#6764,#5857,.T.);
#7996=EDGE_CURVE('',#6764,#6761,#4445,.T.);
#7997=EDGE_CURVE('',#6765,#6765,#5858,.T.);
#7998=EDGE_CURVE('',#6765,#6758,#4446,.T.);
#7999=EDGE_CURVE('',#6766,#6767,#4447,.T.);
#8000=EDGE_CURVE('',#6767,#6768,#4448,.T.);
#8001=EDGE_CURVE('',#6769,#6768,#4449,.T.);
#8002=EDGE_CURVE('',#6766,#6769,#4450,.T.);
#8003=EDGE_CURVE('',#6770,#6766,#4451,.T.);
#8004=EDGE_CURVE('',#6771,#6769,#4452,.T.);
#8005=EDGE_CURVE('',#6770,#6771,#4453,.T.);
#8006=EDGE_CURVE('',#6772,#6770,#4454,.T.);
#8007=EDGE_CURVE('',#6773,#6771,#4455,.T.);
#8008=EDGE_CURVE('',#6772,#6773,#4456,.T.);
#8009=EDGE_CURVE('',#6767,#6772,#4457,.T.);
#8010=EDGE_CURVE('',#6768,#6773,#4458,.T.);
#8011=EDGE_CURVE('',#6774,#6774,#5859,.T.);
#8012=EDGE_CURVE('',#6774,#6775,#4459,.T.);
#8013=EDGE_CURVE('',#6775,#6775,#5860,.T.);
#8014=EDGE_CURVE('',#6776,#6776,#5861,.T.);
#8015=EDGE_CURVE('',#6777,#6777,#5862,.T.);
#8016=EDGE_CURVE('',#6777,#6778,#4460,.T.);
#8017=EDGE_CURVE('',#6778,#6778,#5863,.T.);
#8018=EDGE_CURVE('',#6779,#6779,#5864,.T.);
#8019=EDGE_CURVE('',#6780,#6780,#5865,.T.);
#8020=EDGE_CURVE('',#6780,#6781,#4461,.T.);
#8021=EDGE_CURVE('',#6781,#6781,#5866,.T.);
#8022=EDGE_CURVE('',#6779,#6782,#4462,.T.);
#8023=EDGE_CURVE('',#6782,#6782,#5867,.T.);
#8024=EDGE_CURVE('',#6776,#6783,#4463,.T.);
#8025=EDGE_CURVE('',#6783,#6783,#5868,.T.);
#8026=EDGE_CURVE('',#6784,#6785,#4464,.T.);
#8027=EDGE_CURVE('',#6785,#6786,#4465,.T.);
#8028=EDGE_CURVE('',#6787,#6786,#4466,.T.);
#8029=EDGE_CURVE('',#6784,#6787,#4467,.T.);
#8030=EDGE_CURVE('',#6788,#6784,#4468,.T.);
#8031=EDGE_CURVE('',#6789,#6787,#4469,.T.);
#8032=EDGE_CURVE('',#6788,#6789,#4470,.T.);
#8033=EDGE_CURVE('',#6790,#6788,#4471,.T.);
#8034=EDGE_CURVE('',#6791,#6789,#4472,.T.);
#8035=EDGE_CURVE('',#6790,#6791,#4473,.T.);
#8036=EDGE_CURVE('',#6785,#6790,#4474,.T.);
#8037=EDGE_CURVE('',#6786,#6791,#4475,.T.);
#8038=EDGE_CURVE('',#6792,#6793,#4476,.T.);
#8039=EDGE_CURVE('',#6792,#6793,#5869,.T.);
#8040=EDGE_CURVE('',#6794,#6792,#697,.T.);
#8041=EDGE_CURVE('',#6795,#6794,#5870,.T.);
#8042=EDGE_CURVE('',#6795,#6796,#4477,.T.);
#8043=EDGE_CURVE('',#6796,#6796,#5871,.T.);
#8044=EDGE_CURVE('',#6797,#6795,#5872,.T.);
#8045=EDGE_CURVE('',#6793,#6797,#698,.T.);
#8046=EDGE_CURVE('',#6797,#6794,#4478,.T.);
#8047=EDGE_CURVE('',#6798,#6798,#5873,.T.);
#8048=EDGE_CURVE('',#6798,#6799,#4479,.T.);
#8049=EDGE_CURVE('',#6799,#6799,#5874,.T.);
#8050=EDGE_CURVE('',#6800,#6801,#4480,.T.);
#8051=EDGE_CURVE('',#6801,#6802,#4481,.T.);
#8052=EDGE_CURVE('',#6803,#6802,#4482,.T.);
#8053=EDGE_CURVE('',#6800,#6803,#4483,.T.);
#8054=EDGE_CURVE('',#6804,#6800,#4484,.T.);
#8055=EDGE_CURVE('',#6805,#6803,#4485,.T.);
#8056=EDGE_CURVE('',#6804,#6805,#4486,.T.);
#8057=EDGE_CURVE('',#6806,#6804,#4487,.T.);
#8058=EDGE_CURVE('',#6807,#6805,#4488,.T.);
#8059=EDGE_CURVE('',#6806,#6807,#4489,.T.);
#8060=EDGE_CURVE('',#6801,#6806,#4490,.T.);
#8061=EDGE_CURVE('',#6802,#6807,#4491,.T.);
#8062=EDGE_CURVE('',#6808,#6808,#5875,.T.);
#8063=EDGE_CURVE('',#6808,#6809,#4492,.T.);
#8064=EDGE_CURVE('',#6809,#6809,#5876,.T.);
#8065=EDGE_CURVE('',#6810,#6810,#5877,.T.);
#8066=EDGE_CURVE('',#6810,#6811,#4493,.T.);
#8067=EDGE_CURVE('',#6811,#6811,#5878,.T.);
#8068=EDGE_CURVE('',#6812,#6812,#5879,.T.);
#8069=EDGE_CURVE('',#6812,#6813,#4494,.T.);
#8070=EDGE_CURVE('',#6813,#6813,#5880,.T.);
#8071=EDGE_CURVE('',#6814,#6814,#5881,.T.);
#8072=EDGE_CURVE('',#6814,#6815,#4495,.T.);
#8073=EDGE_CURVE('',#6815,#6815,#5882,.T.);
#8074=EDGE_CURVE('',#6816,#6816,#5883,.T.);
#8075=EDGE_CURVE('',#6816,#6817,#4496,.T.);
#8076=EDGE_CURVE('',#6817,#6817,#5884,.T.);
#8077=EDGE_CURVE('',#6818,#6818,#5885,.T.);
#8078=EDGE_CURVE('',#6818,#6819,#4497,.T.);
#8079=EDGE_CURVE('',#6819,#6819,#5886,.T.);
#8080=EDGE_CURVE('',#6820,#6820,#5887,.T.);
#8081=EDGE_CURVE('',#6820,#6821,#4498,.T.);
#8082=EDGE_CURVE('',#6821,#6821,#5888,.T.);
#8083=EDGE_CURVE('',#6822,#6822,#5889,.T.);
#8084=EDGE_CURVE('',#6822,#6823,#4499,.T.);
#8085=EDGE_CURVE('',#6823,#6823,#5890,.T.);
#8086=EDGE_CURVE('',#6824,#6824,#5891,.T.);
#8087=EDGE_CURVE('',#6824,#6825,#4500,.T.);
#8088=EDGE_CURVE('',#6825,#6825,#5892,.T.);
#8089=EDGE_CURVE('',#6826,#6826,#5893,.T.);
#8090=EDGE_CURVE('',#6826,#6827,#4501,.T.);
#8091=EDGE_CURVE('',#6827,#6827,#5894,.T.);
#8092=EDGE_CURVE('',#6828,#6828,#5895,.T.);
#8093=EDGE_CURVE('',#6828,#6829,#4502,.T.);
#8094=EDGE_CURVE('',#6829,#6829,#5896,.T.);
#8095=EDGE_CURVE('',#6830,#6830,#5897,.T.);
#8096=EDGE_CURVE('',#6830,#6831,#4503,.T.);
#8097=EDGE_CURVE('',#6831,#6831,#5898,.T.);
#8098=EDGE_CURVE('',#6832,#6832,#5899,.T.);
#8099=EDGE_CURVE('',#6832,#6833,#4504,.T.);
#8100=EDGE_CURVE('',#6833,#6833,#5900,.T.);
#8101=EDGE_CURVE('',#6834,#6834,#5901,.T.);
#8102=EDGE_CURVE('',#6834,#6835,#4505,.T.);
#8103=EDGE_CURVE('',#6835,#6835,#5902,.T.);
#8104=EDGE_CURVE('',#6836,#6836,#5903,.T.);
#8105=EDGE_CURVE('',#6836,#6837,#4506,.T.);
#8106=EDGE_CURVE('',#6837,#6837,#5904,.T.);
#8107=EDGE_CURVE('',#6838,#6838,#5905,.T.);
#8108=EDGE_CURVE('',#6838,#6839,#4507,.T.);
#8109=EDGE_CURVE('',#6839,#6839,#5906,.T.);
#8110=EDGE_CURVE('',#6840,#6840,#5907,.T.);
#8111=EDGE_CURVE('',#6840,#6841,#4508,.T.);
#8112=EDGE_CURVE('',#6841,#6841,#5908,.T.);
#8113=EDGE_CURVE('',#6842,#6842,#5909,.T.);
#8114=EDGE_CURVE('',#6842,#6843,#4509,.T.);
#8115=EDGE_CURVE('',#6843,#6843,#5910,.T.);
#8116=EDGE_CURVE('',#6844,#6845,#4510,.T.);
#8117=EDGE_CURVE('',#6845,#6846,#4511,.T.);
#8118=EDGE_CURVE('',#6847,#6846,#4512,.T.);
#8119=EDGE_CURVE('',#6844,#6847,#4513,.T.);
#8120=EDGE_CURVE('',#6848,#6844,#4514,.T.);
#8121=EDGE_CURVE('',#6849,#6847,#4515,.T.);
#8122=EDGE_CURVE('',#6848,#6849,#4516,.T.);
#8123=EDGE_CURVE('',#6850,#6848,#4517,.T.);
#8124=EDGE_CURVE('',#6851,#6849,#4518,.T.);
#8125=EDGE_CURVE('',#6850,#6851,#4519,.T.);
#8126=EDGE_CURVE('',#6845,#6850,#4520,.T.);
#8127=EDGE_CURVE('',#6846,#6851,#4521,.T.);
#8128=EDGE_CURVE('',#6852,#6852,#5911,.T.);
#8129=EDGE_CURVE('',#6852,#6853,#4522,.T.);
#8130=EDGE_CURVE('',#6853,#6853,#5912,.T.);
#8131=EDGE_CURVE('',#6854,#6854,#5913,.T.);
#8132=EDGE_CURVE('',#6855,#6855,#5914,.T.);
#8133=EDGE_CURVE('',#6855,#6856,#4523,.T.);
#8134=EDGE_CURVE('',#6856,#6856,#5915,.T.);
#8135=EDGE_CURVE('',#6857,#6857,#5916,.T.);
#8136=EDGE_CURVE('',#6858,#6858,#5917,.T.);
#8137=EDGE_CURVE('',#6858,#6859,#4524,.T.);
#8138=EDGE_CURVE('',#6859,#6859,#5918,.T.);
#8139=EDGE_CURVE('',#6860,#6860,#5919,.T.);
#8140=EDGE_CURVE('',#6860,#6857,#4525,.T.);
#8141=EDGE_CURVE('',#6861,#6861,#5920,.T.);
#8142=EDGE_CURVE('',#6861,#6854,#4526,.T.);
#8143=EDGE_CURVE('',#6862,#6863,#4527,.T.);
#8144=EDGE_CURVE('',#6863,#6864,#4528,.T.);
#8145=EDGE_CURVE('',#6865,#6864,#4529,.T.);
#8146=EDGE_CURVE('',#6862,#6865,#4530,.T.);
#8147=EDGE_CURVE('',#6866,#6862,#4531,.T.);
#8148=EDGE_CURVE('',#6867,#6865,#4532,.T.);
#8149=EDGE_CURVE('',#6866,#6867,#4533,.T.);
#8150=EDGE_CURVE('',#6868,#6866,#4534,.T.);
#8151=EDGE_CURVE('',#6869,#6867,#4535,.T.);
#8152=EDGE_CURVE('',#6868,#6869,#4536,.T.);
#8153=EDGE_CURVE('',#6863,#6868,#4537,.T.);
#8154=EDGE_CURVE('',#6864,#6869,#4538,.T.);
#8155=EDGE_CURVE('',#6870,#6870,#5921,.T.);
#8156=EDGE_CURVE('',#6870,#6871,#4539,.T.);
#8157=EDGE_CURVE('',#6871,#6871,#5922,.T.);
#8158=EDGE_CURVE('',#6872,#6872,#5923,.T.);
#8159=EDGE_CURVE('',#6873,#6873,#5924,.T.);
#8160=EDGE_CURVE('',#6873,#6874,#4540,.T.);
#8161=EDGE_CURVE('',#6874,#6874,#5925,.T.);
#8162=EDGE_CURVE('',#6875,#6875,#5926,.T.);
#8163=EDGE_CURVE('',#6876,#6876,#5927,.T.);
#8164=EDGE_CURVE('',#6876,#6877,#4541,.T.);
#8165=EDGE_CURVE('',#6877,#6877,#5928,.T.);
#8166=EDGE_CURVE('',#6875,#6878,#4542,.T.);
#8167=EDGE_CURVE('',#6878,#6878,#5929,.T.);
#8168=EDGE_CURVE('',#6872,#6879,#4543,.T.);
#8169=EDGE_CURVE('',#6879,#6879,#5930,.T.);
#8170=EDGE_CURVE('',#6880,#6881,#4544,.T.);
#8171=EDGE_CURVE('',#6881,#6882,#4545,.T.);
#8172=EDGE_CURVE('',#6883,#6882,#4546,.T.);
#8173=EDGE_CURVE('',#6880,#6883,#4547,.T.);
#8174=EDGE_CURVE('',#6884,#6880,#4548,.T.);
#8175=EDGE_CURVE('',#6885,#6883,#4549,.T.);
#8176=EDGE_CURVE('',#6884,#6885,#4550,.T.);
#8177=EDGE_CURVE('',#6886,#6884,#4551,.T.);
#8178=EDGE_CURVE('',#6887,#6885,#4552,.T.);
#8179=EDGE_CURVE('',#6886,#6887,#4553,.T.);
#8180=EDGE_CURVE('',#6881,#6886,#4554,.T.);
#8181=EDGE_CURVE('',#6882,#6887,#4555,.T.);
#8182=EDGE_CURVE('',#6888,#6889,#4556,.T.);
#8183=EDGE_CURVE('',#6888,#6889,#5931,.T.);
#8184=EDGE_CURVE('',#6890,#6888,#699,.T.);
#8185=EDGE_CURVE('',#6891,#6890,#5932,.T.);
#8186=EDGE_CURVE('',#6891,#6892,#4557,.T.);
#8187=EDGE_CURVE('',#6892,#6892,#5933,.T.);
#8188=EDGE_CURVE('',#6893,#6891,#5934,.T.);
#8189=EDGE_CURVE('',#6889,#6893,#700,.T.);
#8190=EDGE_CURVE('',#6893,#6890,#4558,.T.);
#8191=EDGE_CURVE('',#6894,#6894,#5935,.T.);
#8192=EDGE_CURVE('',#6894,#6895,#4559,.T.);
#8193=EDGE_CURVE('',#6895,#6895,#5936,.T.);
#8194=EDGE_CURVE('',#6896,#6897,#4560,.T.);
#8195=EDGE_CURVE('',#6897,#6898,#4561,.T.);
#8196=EDGE_CURVE('',#6899,#6898,#4562,.T.);
#8197=EDGE_CURVE('',#6896,#6899,#4563,.T.);
#8198=EDGE_CURVE('',#6900,#6896,#4564,.T.);
#8199=EDGE_CURVE('',#6901,#6899,#4565,.T.);
#8200=EDGE_CURVE('',#6900,#6901,#4566,.T.);
#8201=EDGE_CURVE('',#6902,#6900,#4567,.T.);
#8202=EDGE_CURVE('',#6903,#6901,#4568,.T.);
#8203=EDGE_CURVE('',#6902,#6903,#4569,.T.);
#8204=EDGE_CURVE('',#6897,#6902,#4570,.T.);
#8205=EDGE_CURVE('',#6898,#6903,#4571,.T.);
#8206=EDGE_CURVE('',#6904,#6904,#5937,.T.);
#8207=EDGE_CURVE('',#6904,#6905,#4572,.T.);
#8208=EDGE_CURVE('',#6905,#6905,#5938,.T.);
#8209=EDGE_CURVE('',#6906,#6906,#5939,.T.);
#8210=EDGE_CURVE('',#6906,#6907,#4573,.T.);
#8211=EDGE_CURVE('',#6907,#6907,#5940,.T.);
#8212=EDGE_CURVE('',#6908,#6908,#5941,.T.);
#8213=EDGE_CURVE('',#6908,#6909,#4574,.T.);
#8214=EDGE_CURVE('',#6909,#6909,#5942,.T.);
#8215=EDGE_CURVE('',#6910,#6910,#5943,.T.);
#8216=EDGE_CURVE('',#6910,#6911,#4575,.T.);
#8217=EDGE_CURVE('',#6911,#6911,#5944,.T.);
#8218=EDGE_CURVE('',#6912,#6912,#5945,.T.);
#8219=EDGE_CURVE('',#6912,#6913,#4576,.T.);
#8220=EDGE_CURVE('',#6913,#6913,#5946,.T.);
#8221=EDGE_CURVE('',#6914,#6914,#5947,.T.);
#8222=EDGE_CURVE('',#6914,#6915,#4577,.T.);
#8223=EDGE_CURVE('',#6915,#6915,#5948,.T.);
#8224=EDGE_CURVE('',#6916,#6916,#5949,.T.);
#8225=EDGE_CURVE('',#6916,#6917,#4578,.T.);
#8226=EDGE_CURVE('',#6917,#6917,#5950,.T.);
#8227=EDGE_CURVE('',#6918,#6918,#5951,.T.);
#8228=EDGE_CURVE('',#6918,#6919,#4579,.T.);
#8229=EDGE_CURVE('',#6919,#6919,#5952,.T.);
#8230=EDGE_CURVE('',#6920,#6920,#5953,.T.);
#8231=EDGE_CURVE('',#6920,#6921,#4580,.T.);
#8232=EDGE_CURVE('',#6921,#6921,#5954,.T.);
#8233=EDGE_CURVE('',#6922,#6922,#5955,.T.);
#8234=EDGE_CURVE('',#6922,#6923,#4581,.T.);
#8235=EDGE_CURVE('',#6923,#6923,#5956,.T.);
#8236=EDGE_CURVE('',#6924,#6924,#5957,.T.);
#8237=EDGE_CURVE('',#6924,#6925,#4582,.T.);
#8238=EDGE_CURVE('',#6925,#6925,#5958,.T.);
#8239=EDGE_CURVE('',#6926,#6926,#5959,.T.);
#8240=EDGE_CURVE('',#6926,#6927,#4583,.T.);
#8241=EDGE_CURVE('',#6927,#6927,#5960,.T.);
#8242=EDGE_CURVE('',#6928,#6928,#5961,.T.);
#8243=EDGE_CURVE('',#6928,#6929,#4584,.T.);
#8244=EDGE_CURVE('',#6929,#6929,#5962,.T.);
#8245=EDGE_CURVE('',#6930,#6930,#5963,.T.);
#8246=EDGE_CURVE('',#6930,#6931,#4585,.T.);
#8247=EDGE_CURVE('',#6931,#6931,#5964,.T.);
#8248=EDGE_CURVE('',#6932,#6932,#5965,.T.);
#8249=EDGE_CURVE('',#6932,#6933,#4586,.T.);
#8250=EDGE_CURVE('',#6933,#6933,#5966,.T.);
#8251=EDGE_CURVE('',#6934,#6935,#5967,.T.);
#8252=EDGE_CURVE('',#6936,#6934,#4587,.T.);
#8253=EDGE_CURVE('',#6937,#6936,#4588,.T.);
#8254=EDGE_CURVE('',#6935,#6937,#4589,.T.);
#8255=EDGE_CURVE('',#6935,#6938,#4590,.T.);
#8256=EDGE_CURVE('',#6939,#6937,#4591,.T.);
#8257=EDGE_CURVE('',#6939,#6938,#4592,.T.);
#8258=EDGE_CURVE('',#6938,#6940,#5968,.T.);
#8259=EDGE_CURVE('',#6941,#6939,#4593,.T.);
#8260=EDGE_CURVE('',#6940,#6941,#4594,.T.);
#8261=EDGE_CURVE('',#6940,#6934,#4595,.T.);
#8262=EDGE_CURVE('',#6941,#6936,#4596,.T.);
#8263=EDGE_CURVE('',#6942,#6942,#5969,.T.);
#8264=EDGE_CURVE('',#6943,#6943,#5970,.T.);
#8265=EDGE_CURVE('',#6944,#6944,#5971,.T.);
#8266=EDGE_CURVE('',#6944,#6942,#4597,.T.);
#8267=EDGE_CURVE('',#6945,#6945,#5972,.T.);
#8268=EDGE_CURVE('',#6946,#6946,#5973,.T.);
#8269=EDGE_CURVE('',#6946,#6945,#4598,.T.);
#8270=EDGE_CURVE('',#6947,#6947,#5974,.T.);
#8271=EDGE_CURVE('',#6948,#6948,#5975,.T.);
#8272=EDGE_CURVE('',#6948,#6947,#4599,.T.);
#8273=EDGE_CURVE('',#6949,#6949,#5976,.T.);
#8274=EDGE_CURVE('',#6950,#6950,#5977,.T.);
#8275=EDGE_CURVE('',#6950,#6949,#4600,.T.);
#8276=EDGE_CURVE('',#6951,#6951,#5978,.T.);
#8277=EDGE_CURVE('',#6952,#6952,#5979,.T.);
#8278=EDGE_CURVE('',#6952,#6951,#4601,.T.);
#8279=EDGE_CURVE('',#6953,#6953,#5980,.T.);
#8280=EDGE_CURVE('',#6953,#6943,#4602,.T.);
#8281=EDGE_CURVE('',#6954,#6955,#5981,.T.);
#8282=EDGE_CURVE('',#6956,#6954,#4603,.T.);
#8283=EDGE_CURVE('',#6957,#6956,#5982,.T.);
#8284=EDGE_CURVE('',#6955,#6957,#4604,.T.);
#8285=EDGE_CURVE('',#6955,#6958,#4605,.T.);
#8286=EDGE_CURVE('',#6959,#6957,#4606,.T.);
#8287=EDGE_CURVE('',#6959,#6958,#4607,.T.);
#8288=EDGE_CURVE('',#6958,#6960,#5983,.T.);
#8289=EDGE_CURVE('',#6961,#6959,#5984,.T.);
#8290=EDGE_CURVE('',#6960,#6961,#4608,.T.);
#8291=EDGE_CURVE('',#6960,#6954,#4609,.T.);
#8292=EDGE_CURVE('',#6956,#6961,#4610,.T.);
#8293=EDGE_CURVE('',#6962,#6962,#5985,.T.);
#8294=EDGE_CURVE('',#6963,#6963,#5986,.T.);
#8295=EDGE_CURVE('',#6964,#6964,#5987,.T.);
#8296=EDGE_CURVE('',#6964,#6962,#4611,.T.);
#8297=EDGE_CURVE('',#6965,#6965,#5988,.T.);
#8298=EDGE_CURVE('',#6965,#6963,#4612,.T.);
#8299=EDGE_CURVE('',#6966,#6966,#5989,.T.);
#8300=EDGE_CURVE('',#6967,#6968,#4613,.T.);
#8301=EDGE_CURVE('',#6967,#6969,#4614,.T.);
#8302=EDGE_CURVE('',#6969,#6970,#4615,.T.);
#8303=EDGE_CURVE('',#6968,#6970,#4616,.T.);
#8304=EDGE_CURVE('',#6971,#6967,#4617,.T.);
#8305=EDGE_CURVE('',#6971,#6972,#4618,.T.);
#8306=EDGE_CURVE('',#6972,#6969,#4619,.T.);
#8307=EDGE_CURVE('',#6973,#6971,#4620,.T.);
#8308=EDGE_CURVE('',#6973,#6974,#4621,.T.);
#8309=EDGE_CURVE('',#6974,#6972,#4622,.T.);
#8310=EDGE_CURVE('',#6975,#6973,#4623,.T.);
#8311=EDGE_CURVE('',#6975,#6976,#4624,.T.);
#8312=EDGE_CURVE('',#6976,#6974,#4625,.T.);
#8313=EDGE_CURVE('',#6977,#6975,#4626,.T.);
#8314=EDGE_CURVE('',#6977,#6978,#4627,.T.);
#8315=EDGE_CURVE('',#6978,#6976,#4628,.T.);
#8316=EDGE_CURVE('',#6968,#6977,#4629,.T.);
#8317=EDGE_CURVE('',#6970,#6978,#4630,.T.);
#8318=EDGE_CURVE('',#6979,#6979,#5990,.T.);
#8319=EDGE_CURVE('',#6980,#6980,#5991,.T.);
#8320=EDGE_CURVE('',#6980,#6979,#4631,.T.);
#8321=EDGE_CURVE('',#6966,#6980,#4632,.T.);
#8322=EDGE_CURVE('',#6981,#6981,#5992,.T.);
#8323=EDGE_CURVE('',#6981,#6982,#4633,.T.);
#8324=EDGE_CURVE('',#6982,#6982,#5993,.T.);
#8325=EDGE_CURVE('',#6983,#6984,#4634,.T.);
#8326=EDGE_CURVE('',#6983,#6985,#5994,.T.);
#8327=EDGE_CURVE('',#6986,#6985,#4635,.T.);
#8328=EDGE_CURVE('',#6984,#6986,#5995,.T.);
#8329=EDGE_CURVE('',#6987,#6988,#4636,.T.);
#8330=EDGE_CURVE('',#6989,#6987,#5996,.T.);
#8331=EDGE_CURVE('',#6990,#6989,#4637,.T.);
#8332=EDGE_CURVE('',#6990,#6988,#5997,.T.);
#8333=EDGE_CURVE('',#6991,#6989,#4638,.T.);
#8334=EDGE_CURVE('',#6991,#6992,#4639,.T.);
#8335=EDGE_CURVE('',#6992,#6990,#4640,.T.);
#8336=EDGE_CURVE('',#6988,#6993,#4641,.T.);
#8337=EDGE_CURVE('',#6993,#6994,#4642,.T.);
#8338=EDGE_CURVE('',#6987,#6994,#4643,.T.);
#8339=EDGE_CURVE('',#6985,#6995,#4644,.T.);
#8340=EDGE_CURVE('',#6995,#6996,#4645,.T.);
#8341=EDGE_CURVE('',#6986,#6996,#4646,.T.);
#8342=EDGE_CURVE('',#6997,#6997,#5998,.T.);
#8343=EDGE_CURVE('',#6997,#6998,#4647,.T.);
#8344=EDGE_CURVE('',#6998,#6998,#5999,.T.);
#8345=EDGE_CURVE('',#6996,#6991,#6000,.T.);
#8346=EDGE_CURVE('',#6995,#6992,#6001,.T.);
#8347=EDGE_CURVE('',#6999,#6983,#4648,.T.);
#8348=EDGE_CURVE('',#6993,#6999,#6002,.T.);
#8349=EDGE_CURVE('',#7000,#7000,#6003,.T.);
#8350=EDGE_CURVE('',#7001,#6984,#4649,.T.);
#8351=EDGE_CURVE('',#7001,#6999,#4650,.T.);
#8352=EDGE_CURVE('',#7000,#7002,#4651,.T.);
#8353=EDGE_CURVE('',#7002,#7002,#6004,.T.);
#8354=EDGE_CURVE('',#6994,#7001,#6005,.T.);
#8355=EDGE_CURVE('',#7003,#7003,#6006,.T.);
#8356=EDGE_CURVE('',#7003,#7004,#4652,.T.);
#8357=EDGE_CURVE('',#7004,#7004,#6007,.T.);
#8358=EDGE_CURVE('',#7005,#7005,#6008,.T.);
#8359=EDGE_CURVE('',#7005,#7006,#4653,.T.);
#8360=EDGE_CURVE('',#7006,#7006,#6009,.T.);
#8361=EDGE_CURVE('',#7007,#7007,#6010,.T.);
#8362=EDGE_CURVE('',#7007,#7008,#4654,.T.);
#8363=EDGE_CURVE('',#7008,#7008,#6011,.T.);
#8364=EDGE_CURVE('',#7009,#7009,#6012,.T.);
#8365=EDGE_CURVE('',#7009,#7010,#4655,.T.);
#8366=EDGE_CURVE('',#7010,#7010,#6013,.T.);
#8367=EDGE_CURVE('',#7011,#7011,#6014,.T.);
#8368=EDGE_CURVE('',#7011,#7012,#4656,.T.);
#8369=EDGE_CURVE('',#7012,#7012,#6015,.T.);
#8370=EDGE_CURVE('',#7013,#7013,#6016,.T.);
#8371=EDGE_CURVE('',#7013,#7014,#4657,.T.);
#8372=EDGE_CURVE('',#7014,#7014,#6017,.T.);
#8373=EDGE_CURVE('',#7015,#7015,#6018,.T.);
#8374=EDGE_CURVE('',#7015,#7016,#4658,.T.);
#8375=EDGE_CURVE('',#7016,#7016,#6019,.T.);
#8376=EDGE_CURVE('',#7017,#7018,#4659,.T.);
#8377=EDGE_CURVE('',#7017,#7019,#6020,.T.);
#8378=EDGE_CURVE('',#7020,#7019,#4660,.T.);
#8379=EDGE_CURVE('',#7018,#7020,#6021,.T.);
#8380=EDGE_CURVE('',#7021,#7022,#4661,.T.);
#8381=EDGE_CURVE('',#7023,#7021,#6022,.T.);
#8382=EDGE_CURVE('',#7024,#7023,#4662,.T.);
#8383=EDGE_CURVE('',#7024,#7022,#6023,.T.);
#8384=EDGE_CURVE('',#7025,#7023,#4663,.T.);
#8385=EDGE_CURVE('',#7025,#7026,#4664,.T.);
#8386=EDGE_CURVE('',#7026,#7024,#4665,.T.);
#8387=EDGE_CURVE('',#7022,#7027,#4666,.T.);
#8388=EDGE_CURVE('',#7027,#7028,#4667,.T.);
#8389=EDGE_CURVE('',#7021,#7028,#4668,.T.);
#8390=EDGE_CURVE('',#7019,#7029,#4669,.T.);
#8391=EDGE_CURVE('',#7029,#7030,#4670,.T.);
#8392=EDGE_CURVE('',#7020,#7030,#4671,.T.);
#8393=EDGE_CURVE('',#7031,#7031,#6024,.T.);
#8394=EDGE_CURVE('',#7031,#7032,#4672,.T.);
#8395=EDGE_CURVE('',#7032,#7032,#6025,.T.);
#8396=EDGE_CURVE('',#7030,#7025,#6026,.T.);
#8397=EDGE_CURVE('',#7029,#7026,#6027,.T.);
#8398=EDGE_CURVE('',#7033,#7017,#4673,.T.);
#8399=EDGE_CURVE('',#7027,#7033,#6028,.T.);
#8400=EDGE_CURVE('',#7034,#7034,#6029,.T.);
#8401=EDGE_CURVE('',#7035,#7018,#4674,.T.);
#8402=EDGE_CURVE('',#7035,#7033,#4675,.T.);
#8403=EDGE_CURVE('',#7034,#7036,#4676,.T.);
#8404=EDGE_CURVE('',#7036,#7036,#6030,.T.);
#8405=EDGE_CURVE('',#7028,#7035,#6031,.T.);
#8406=EDGE_CURVE('',#7037,#7037,#6032,.T.);
#8407=EDGE_CURVE('',#7037,#7038,#4677,.T.);
#8408=EDGE_CURVE('',#7038,#7038,#6033,.T.);
#8409=EDGE_CURVE('',#7039,#7039,#6034,.T.);
#8410=EDGE_CURVE('',#7039,#7040,#4678,.T.);
#8411=EDGE_CURVE('',#7040,#7040,#6035,.T.);
#8412=EDGE_CURVE('',#7041,#7041,#6036,.T.);
#8413=EDGE_CURVE('',#7041,#7042,#4679,.T.);
#8414=EDGE_CURVE('',#7042,#7042,#6037,.T.);
#8415=EDGE_CURVE('',#7043,#7043,#6038,.T.);
#8416=EDGE_CURVE('',#7043,#7044,#4680,.T.);
#8417=EDGE_CURVE('',#7044,#7044,#6039,.T.);
#8418=EDGE_CURVE('',#7045,#7045,#6040,.T.);
#8419=EDGE_CURVE('',#7045,#7046,#4681,.T.);
#8420=EDGE_CURVE('',#7046,#7046,#6041,.T.);
#8421=EDGE_CURVE('',#7047,#7047,#6042,.T.);
#8422=EDGE_CURVE('',#7047,#7048,#4682,.T.);
#8423=EDGE_CURVE('',#7048,#7048,#6043,.T.);
#8424=EDGE_CURVE('',#7049,#7049,#6044,.T.);
#8425=EDGE_CURVE('',#7049,#7050,#4683,.T.);
#8426=EDGE_CURVE('',#7050,#7050,#6045,.T.);
#8427=EDGE_CURVE('',#7051,#7051,#6046,.T.);
#8428=EDGE_CURVE('',#7051,#7052,#4684,.T.);
#8429=EDGE_CURVE('',#7052,#7052,#6047,.T.);
#8430=EDGE_CURVE('',#7053,#7053,#6048,.T.);
#8431=EDGE_CURVE('',#7053,#7054,#4685,.T.);
#8432=EDGE_CURVE('',#7054,#7054,#6049,.T.);
#8433=EDGE_CURVE('',#7055,#7055,#6050,.T.);
#8434=EDGE_CURVE('',#7055,#7056,#4686,.T.);
#8435=EDGE_CURVE('',#7056,#7056,#6051,.T.);
#8436=EDGE_CURVE('',#7057,#7057,#6052,.T.);
#8437=EDGE_CURVE('',#7057,#7058,#4687,.T.);
#8438=EDGE_CURVE('',#7058,#7058,#6053,.T.);
#8439=EDGE_CURVE('',#7059,#7059,#6054,.T.);
#8440=EDGE_CURVE('',#7059,#7060,#4688,.T.);
#8441=EDGE_CURVE('',#7060,#7060,#6055,.T.);
#8442=EDGE_CURVE('',#7061,#7061,#6056,.T.);
#8443=EDGE_CURVE('',#7061,#7062,#4689,.T.);
#8444=EDGE_CURVE('',#7062,#7062,#6057,.T.);
#8445=EDGE_CURVE('',#7063,#7063,#6058,.T.);
#8446=EDGE_CURVE('',#7063,#7064,#4690,.T.);
#8447=EDGE_CURVE('',#7064,#7064,#6059,.T.);
#8448=EDGE_CURVE('',#7065,#7065,#6060,.T.);
#8449=EDGE_CURVE('',#7065,#7066,#4691,.T.);
#8450=EDGE_CURVE('',#7066,#7066,#6061,.T.);
#8451=EDGE_CURVE('',#7067,#7067,#6062,.T.);
#8452=EDGE_CURVE('',#7067,#7068,#4692,.T.);
#8453=EDGE_CURVE('',#7068,#7068,#6063,.T.);
#8454=EDGE_CURVE('',#7069,#7069,#6064,.T.);
#8455=EDGE_CURVE('',#7069,#7070,#4693,.T.);
#8456=EDGE_CURVE('',#7070,#7070,#6065,.T.);
#8457=EDGE_CURVE('',#7071,#7071,#6066,.T.);
#8458=EDGE_CURVE('',#7071,#7072,#4694,.T.);
#8459=EDGE_CURVE('',#7072,#7072,#6067,.T.);
#8460=EDGE_CURVE('',#7073,#7073,#6068,.T.);
#8461=EDGE_CURVE('',#7073,#7074,#4695,.T.);
#8462=EDGE_CURVE('',#7074,#7074,#6069,.T.);
#8463=EDGE_CURVE('',#7075,#7075,#6070,.T.);
#8464=EDGE_CURVE('',#7075,#7076,#4696,.T.);
#8465=EDGE_CURVE('',#7076,#7076,#6071,.T.);
#8466=EDGE_CURVE('',#7077,#7077,#6072,.T.);
#8467=EDGE_CURVE('',#7077,#7078,#4697,.T.);
#8468=EDGE_CURVE('',#7078,#7078,#6073,.T.);
#8469=EDGE_CURVE('',#7079,#7079,#6074,.T.);
#8470=EDGE_CURVE('',#7079,#7080,#4698,.T.);
#8471=EDGE_CURVE('',#7080,#7080,#6075,.T.);
#8472=EDGE_CURVE('',#7081,#7081,#6076,.T.);
#8473=EDGE_CURVE('',#7081,#7082,#4699,.T.);
#8474=EDGE_CURVE('',#7082,#7082,#6077,.T.);
#8475=EDGE_CURVE('',#7083,#7083,#6078,.T.);
#8476=EDGE_CURVE('',#7084,#7084,#6079,.T.);
#8477=EDGE_CURVE('',#7084,#7083,#4700,.T.);
#8478=EDGE_CURVE('',#7085,#7085,#6080,.T.);
#8479=EDGE_CURVE('',#7085,#7084,#4701,.T.);
#8480=EDGE_CURVE('',#7086,#7086,#6081,.T.);
#8481=EDGE_CURVE('',#7086,#7085,#4702,.T.);
#8482=EDGE_CURVE('',#7087,#7087,#6082,.T.);
#8483=EDGE_CURVE('',#7088,#7088,#6083,.F.);
#8484=EDGE_CURVE('',#7088,#7087,#4703,.T.);
#8485=EDGE_CURVE('',#7089,#7089,#6084,.F.);
#8486=EDGE_CURVE('',#7089,#7088,#4704,.T.);
#8487=EDGE_CURVE('',#7090,#7090,#6085,.T.);
#8488=EDGE_CURVE('',#7090,#7089,#4705,.T.);
#8489=EDGE_CURVE('',#7091,#7092,#4706,.T.);
#8490=EDGE_CURVE('',#7092,#7093,#4707,.T.);
#8491=EDGE_CURVE('',#7093,#7094,#4708,.T.);
#8492=EDGE_CURVE('',#7091,#7094,#4709,.T.);
#8493=EDGE_CURVE('',#7092,#7095,#4710,.T.);
#8494=EDGE_CURVE('',#7095,#7096,#4711,.T.);
#8495=EDGE_CURVE('',#7096,#7093,#4712,.T.);
#8496=EDGE_CURVE('',#7095,#7097,#4713,.T.);
#8497=EDGE_CURVE('',#7097,#7098,#4714,.T.);
#8498=EDGE_CURVE('',#7098,#7096,#4715,.T.);
#8499=EDGE_CURVE('',#7097,#7099,#4716,.T.);
#8500=EDGE_CURVE('',#7099,#7100,#4717,.T.);
#8501=EDGE_CURVE('',#7100,#7098,#4718,.T.);
#8502=EDGE_CURVE('',#7099,#7101,#4719,.T.);
#8503=EDGE_CURVE('',#7101,#7102,#4720,.T.);
#8504=EDGE_CURVE('',#7102,#7100,#4721,.T.);
#8505=EDGE_CURVE('',#7101,#7091,#4722,.T.);
#8506=EDGE_CURVE('',#7094,#7102,#4723,.T.);
#8507=EDGE_CURVE('',#7103,#7103,#6086,.T.);
#8508=EDGE_CURVE('',#7103,#7104,#4724,.T.);
#8509=EDGE_CURVE('',#7104,#7104,#6087,.T.);
#8510=EDGE_CURVE('',#7105,#7105,#6088,.T.);
#8511=EDGE_CURVE('',#7105,#7106,#4725,.T.);
#8512=EDGE_CURVE('',#7106,#7106,#6089,.T.);
#8513=EDGE_CURVE('',#7107,#7107,#6090,.T.);
#8514=EDGE_CURVE('',#7107,#7108,#4726,.T.);
#8515=EDGE_CURVE('',#7108,#7108,#6091,.T.);
#8516=EDGE_CURVE('',#7109,#7109,#6092,.T.);
#8517=EDGE_CURVE('',#7109,#7110,#4727,.T.);
#8518=EDGE_CURVE('',#7110,#7110,#6093,.T.);
#8519=EDGE_CURVE('',#7111,#7111,#6094,.T.);
#8520=EDGE_CURVE('',#7111,#7112,#4728,.T.);
#8521=EDGE_CURVE('',#7112,#7112,#6095,.T.);
#8522=EDGE_CURVE('',#7113,#7114,#4729,.T.);
#8523=EDGE_CURVE('',#7115,#7113,#6096,.T.);
#8524=EDGE_CURVE('',#7116,#7115,#4730,.T.);
#8525=EDGE_CURVE('',#7116,#7114,#6097,.T.);
#8526=EDGE_CURVE('',#7117,#7118,#4731,.T.);
#8527=EDGE_CURVE('',#7117,#7119,#6098,.T.);
#8528=EDGE_CURVE('',#7120,#7119,#4732,.T.);
#8529=EDGE_CURVE('',#7118,#7120,#6099,.T.);
#8530=EDGE_CURVE('',#7119,#7121,#4733,.T.);
#8531=EDGE_CURVE('',#7121,#7122,#4734,.T.);
#8532=EDGE_CURVE('',#7120,#7122,#4735,.T.);
#8533=EDGE_CURVE('',#7122,#7123,#6100,.T.);
#8534=EDGE_CURVE('',#7123,#7115,#4736,.T.);
#8535=EDGE_CURVE('',#7113,#7124,#4737,.T.);
#8536=EDGE_CURVE('',#7124,#7125,#6101,.T.);
#8537=EDGE_CURVE('',#7125,#7118,#4738,.T.);
#8538=EDGE_CURVE('',#7126,#7126,#6102,.T.);
#8539=EDGE_CURVE('',#7127,#7127,#6103,.T.);
#8540=EDGE_CURVE('',#7123,#7128,#4739,.T.);
#8541=EDGE_CURVE('',#7128,#7116,#4740,.T.);
#8542=EDGE_CURVE('',#7129,#7129,#6104,.T.);
#8543=EDGE_CURVE('',#7129,#7126,#4741,.T.);
#8544=EDGE_CURVE('',#7130,#7124,#4742,.T.);
#8545=EDGE_CURVE('',#7130,#7131,#6105,.T.);
#8546=EDGE_CURVE('',#7125,#7131,#4743,.T.);
#8547=EDGE_CURVE('',#7114,#7130,#4744,.T.);
#8548=EDGE_CURVE('',#7132,#7132,#6106,.T.);
#8549=EDGE_CURVE('',#7132,#7127,#4745,.T.);
#8550=EDGE_CURVE('',#7121,#7128,#6107,.T.);
#8551=EDGE_CURVE('',#7131,#7117,#4746,.T.);
#8552=EDGE_CURVE('',#7133,#7133,#6108,.T.);
#8553=EDGE_CURVE('',#7133,#7134,#4747,.T.);
#8554=EDGE_CURVE('',#7134,#7134,#6109,.T.);
#8555=EDGE_CURVE('',#7135,#7135,#6110,.T.);
#8556=EDGE_CURVE('',#7135,#7136,#4748,.T.);
#8557=EDGE_CURVE('',#7136,#7136,#6111,.T.);
#8558=EDGE_CURVE('',#7137,#7137,#6112,.T.);
#8559=EDGE_CURVE('',#7137,#7138,#4749,.T.);
#8560=EDGE_CURVE('',#7138,#7138,#6113,.T.);
#8561=EDGE_CURVE('',#7139,#7139,#6114,.T.);
#8562=EDGE_CURVE('',#7139,#7140,#4750,.T.);
#8563=EDGE_CURVE('',#7140,#7140,#6115,.T.);
#8564=EDGE_CURVE('',#7141,#7141,#6116,.T.);
#8565=EDGE_CURVE('',#7141,#7142,#4751,.T.);
#8566=EDGE_CURVE('',#7142,#7142,#6117,.T.);
#8567=EDGE_CURVE('',#7143,#7143,#6118,.T.);
#8568=EDGE_CURVE('',#7143,#7144,#4752,.T.);
#8569=EDGE_CURVE('',#7144,#7144,#6119,.T.);
#8570=EDGE_CURVE('',#7145,#7145,#6120,.T.);
#8571=EDGE_CURVE('',#7145,#7146,#4753,.T.);
#8572=EDGE_CURVE('',#7146,#7146,#6121,.T.);
#8573=EDGE_CURVE('',#7147,#7147,#6122,.T.);
#8574=EDGE_CURVE('',#7147,#7148,#4754,.T.);
#8575=EDGE_CURVE('',#7148,#7148,#6123,.T.);
#8576=EDGE_CURVE('',#7149,#7149,#6124,.T.);
#8577=EDGE_CURVE('',#7149,#7150,#4755,.T.);
#8578=EDGE_CURVE('',#7150,#7150,#6125,.T.);
#8579=EDGE_CURVE('',#7151,#7151,#6126,.T.);
#8580=EDGE_CURVE('',#7151,#7152,#4756,.T.);
#8581=EDGE_CURVE('',#7152,#7152,#6127,.T.);
#8582=EDGE_CURVE('',#7153,#7153,#6128,.T.);
#8583=EDGE_CURVE('',#7154,#7154,#6129,.T.);
#8584=EDGE_CURVE('',#7153,#7155,#4757,.T.);
#8585=EDGE_CURVE('',#7155,#7155,#6130,.T.);
#8586=EDGE_CURVE('',#7156,#7156,#6131,.T.);
#8587=EDGE_CURVE('',#7156,#7154,#4758,.T.);
#8588=EDGE_CURVE('',#7157,#7157,#6132,.T.);
#8589=EDGE_CURVE('',#7158,#7158,#6133,.T.);
#8590=EDGE_CURVE('',#7157,#7159,#4759,.T.);
#8591=EDGE_CURVE('',#7159,#7159,#6134,.T.);
#8592=EDGE_CURVE('',#7160,#7160,#6135,.T.);
#8593=EDGE_CURVE('',#7160,#7158,#4760,.T.);
#8594=EDGE_CURVE('',#7161,#7161,#6136,.T.);
#8595=EDGE_CURVE('',#7162,#7162,#6137,.T.);
#8596=EDGE_CURVE('',#7161,#7163,#4761,.T.);
#8597=EDGE_CURVE('',#7163,#7163,#6138,.T.);
#8598=EDGE_CURVE('',#7164,#7164,#6139,.T.);
#8599=EDGE_CURVE('',#7164,#7162,#4762,.T.);
#8600=EDGE_CURVE('',#7165,#7165,#6140,.T.);
#8601=EDGE_CURVE('',#7166,#7166,#6141,.T.);
#8602=EDGE_CURVE('',#7165,#7167,#4763,.T.);
#8603=EDGE_CURVE('',#7167,#7167,#6142,.T.);
#8604=EDGE_CURVE('',#7168,#7168,#6143,.T.);
#8605=EDGE_CURVE('',#7168,#7166,#4764,.T.);
#8606=EDGE_CURVE('',#7169,#7169,#6144,.T.);
#8607=EDGE_CURVE('',#7169,#7170,#4765,.T.);
#8608=EDGE_CURVE('',#7170,#7170,#6145,.T.);
#8609=EDGE_CURVE('',#7171,#7171,#6146,.T.);
#8610=EDGE_CURVE('',#7171,#7172,#4766,.T.);
#8611=EDGE_CURVE('',#7172,#7172,#6147,.T.);
#8612=EDGE_CURVE('',#7173,#7173,#6148,.T.);
#8613=EDGE_CURVE('',#7173,#7174,#4767,.T.);
#8614=EDGE_CURVE('',#7174,#7174,#6149,.T.);
#8615=EDGE_CURVE('',#7175,#7175,#6150,.T.);
#8616=EDGE_CURVE('',#7175,#7176,#4768,.T.);
#8617=EDGE_CURVE('',#7176,#7176,#6151,.T.);
#8618=EDGE_CURVE('',#7177,#7177,#6152,.T.);
#8619=EDGE_CURVE('',#7177,#7178,#4769,.T.);
#8620=EDGE_CURVE('',#7178,#7178,#6153,.T.);
#8621=EDGE_CURVE('',#7179,#7179,#6154,.T.);
#8622=EDGE_CURVE('',#7179,#7180,#4770,.T.);
#8623=EDGE_CURVE('',#7180,#7180,#6155,.T.);
#8624=EDGE_CURVE('',#7181,#7181,#6156,.T.);
#8625=EDGE_CURVE('',#7182,#7182,#6157,.T.);
#8626=EDGE_CURVE('',#7183,#7183,#6158,.T.);
#8627=EDGE_CURVE('',#7183,#7181,#4771,.T.);
#8628=EDGE_CURVE('',#7182,#7184,#4772,.T.);
#8629=EDGE_CURVE('',#7184,#7184,#6159,.T.);
#8630=EDGE_CURVE('',#7185,#7185,#6160,.T.);
#8631=EDGE_CURVE('',#7186,#7186,#6161,.T.);
#8632=EDGE_CURVE('',#7187,#7187,#6162,.T.);
#8633=EDGE_CURVE('',#7187,#7185,#4773,.T.);
#8634=EDGE_CURVE('',#7186,#7188,#4774,.T.);
#8635=EDGE_CURVE('',#7188,#7188,#6163,.T.);
#8636=EDGE_CURVE('',#7189,#7189,#6164,.T.);
#8637=EDGE_CURVE('',#7190,#7190,#6165,.T.);
#8638=EDGE_CURVE('',#7191,#7191,#6166,.T.);
#8639=EDGE_CURVE('',#7191,#7189,#4775,.T.);
#8640=EDGE_CURVE('',#7190,#7192,#4776,.T.);
#8641=EDGE_CURVE('',#7192,#7192,#6167,.T.);
#8642=EDGE_CURVE('',#7193,#7193,#6168,.T.);
#8643=EDGE_CURVE('',#7194,#7194,#6169,.T.);
#8644=EDGE_CURVE('',#7195,#7195,#6170,.T.);
#8645=EDGE_CURVE('',#7195,#7193,#4777,.T.);
#8646=EDGE_CURVE('',#7194,#7196,#4778,.T.);
#8647=EDGE_CURVE('',#7196,#7196,#6171,.T.);
#8648=EDGE_CURVE('',#7197,#7197,#6172,.T.);
#8649=EDGE_CURVE('',#7197,#7198,#4779,.T.);
#8650=EDGE_CURVE('',#7198,#7198,#6173,.T.);
#8651=EDGE_CURVE('',#7199,#7199,#6174,.T.);
#8652=EDGE_CURVE('',#7199,#7200,#4780,.T.);
#8653=EDGE_CURVE('',#7200,#7200,#6175,.T.);
#8654=EDGE_CURVE('',#7201,#7201,#6176,.T.);
#8655=EDGE_CURVE('',#7201,#7202,#4781,.T.);
#8656=EDGE_CURVE('',#7202,#7202,#6177,.T.);
#8657=EDGE_CURVE('',#7203,#7203,#6178,.T.);
#8658=EDGE_CURVE('',#7203,#7204,#4782,.T.);
#8659=EDGE_CURVE('',#7204,#7204,#6179,.T.);
#8660=EDGE_CURVE('',#7205,#7205,#6180,.T.);
#8661=EDGE_CURVE('',#7205,#7206,#4783,.T.);
#8662=EDGE_CURVE('',#7206,#7206,#6181,.T.);
#8663=EDGE_CURVE('',#7207,#7208,#4784,.T.);
#8664=EDGE_CURVE('',#7209,#7207,#6182,.T.);
#8665=EDGE_CURVE('',#7210,#7209,#4785,.T.);
#8666=EDGE_CURVE('',#7210,#7208,#6183,.T.);
#8667=EDGE_CURVE('',#7211,#7212,#4786,.T.);
#8668=EDGE_CURVE('',#7211,#7213,#6184,.T.);
#8669=EDGE_CURVE('',#7214,#7213,#4787,.T.);
#8670=EDGE_CURVE('',#7212,#7214,#6185,.T.);
#8671=EDGE_CURVE('',#7213,#7215,#4788,.T.);
#8672=EDGE_CURVE('',#7215,#7216,#4789,.T.);
#8673=EDGE_CURVE('',#7214,#7216,#4790,.T.);
#8674=EDGE_CURVE('',#7216,#7217,#6186,.T.);
#8675=EDGE_CURVE('',#7217,#7209,#4791,.T.);
#8676=EDGE_CURVE('',#7207,#7218,#4792,.T.);
#8677=EDGE_CURVE('',#7218,#7219,#6187,.T.);
#8678=EDGE_CURVE('',#7219,#7212,#4793,.T.);
#8679=EDGE_CURVE('',#7220,#7220,#6188,.T.);
#8680=EDGE_CURVE('',#7221,#7221,#6189,.T.);
#8681=EDGE_CURVE('',#7217,#7222,#4794,.T.);
#8682=EDGE_CURVE('',#7222,#7210,#4795,.T.);
#8683=EDGE_CURVE('',#7223,#7223,#6190,.T.);
#8684=EDGE_CURVE('',#7223,#7220,#4796,.T.);
#8685=EDGE_CURVE('',#7224,#7218,#4797,.T.);
#8686=EDGE_CURVE('',#7224,#7225,#6191,.T.);
#8687=EDGE_CURVE('',#7219,#7225,#4798,.T.);
#8688=EDGE_CURVE('',#7208,#7224,#4799,.T.);
#8689=EDGE_CURVE('',#7226,#7226,#6192,.T.);
#8690=EDGE_CURVE('',#7226,#7221,#4800,.T.);
#8691=EDGE_CURVE('',#7215,#7222,#6193,.T.);
#8692=EDGE_CURVE('',#7225,#7211,#4801,.T.);
#8693=EDGE_CURVE('',#7227,#7227,#6194,.T.);
#8694=EDGE_CURVE('',#7227,#7228,#4802,.T.);
#8695=EDGE_CURVE('',#7228,#7228,#6195,.T.);
#8696=EDGE_CURVE('',#7229,#7229,#6196,.T.);
#8697=EDGE_CURVE('',#7229,#7230,#4803,.T.);
#8698=EDGE_CURVE('',#7230,#7230,#6197,.T.);
#8699=EDGE_CURVE('',#7231,#7231,#6198,.T.);
#8700=EDGE_CURVE('',#7231,#7232,#4804,.T.);
#8701=EDGE_CURVE('',#7232,#7232,#6199,.T.);
#8702=EDGE_CURVE('',#7233,#7233,#6200,.T.);
#8703=EDGE_CURVE('',#7233,#7234,#4805,.T.);
#8704=EDGE_CURVE('',#7234,#7234,#6201,.T.);
#8705=EDGE_CURVE('',#7235,#7235,#6202,.T.);
#8706=EDGE_CURVE('',#7235,#7236,#4806,.T.);
#8707=EDGE_CURVE('',#7236,#7236,#6203,.T.);
#8708=EDGE_CURVE('',#7237,#7237,#6204,.T.);
#8709=EDGE_CURVE('',#7237,#7238,#4807,.T.);
#8710=EDGE_CURVE('',#7238,#7238,#6205,.T.);
#8711=EDGE_CURVE('',#7239,#7239,#6206,.T.);
#8712=EDGE_CURVE('',#7239,#7240,#4808,.T.);
#8713=EDGE_CURVE('',#7240,#7240,#6207,.T.);
#8714=EDGE_CURVE('',#7241,#7241,#6208,.T.);
#8715=EDGE_CURVE('',#7241,#7242,#4809,.T.);
#8716=EDGE_CURVE('',#7242,#7242,#6209,.T.);
#8717=EDGE_CURVE('',#7243,#7243,#6210,.T.);
#8718=EDGE_CURVE('',#7243,#7244,#4810,.T.);
#8719=EDGE_CURVE('',#7244,#7244,#6211,.T.);
#8720=EDGE_CURVE('',#7245,#7245,#6212,.T.);
#8721=EDGE_CURVE('',#7245,#7246,#4811,.T.);
#8722=EDGE_CURVE('',#7246,#7246,#6213,.T.);
#8723=EDGE_CURVE('',#7247,#7247,#6214,.T.);
#8724=EDGE_CURVE('',#7248,#7248,#6215,.T.);
#8725=EDGE_CURVE('',#7247,#7249,#4812,.T.);
#8726=EDGE_CURVE('',#7249,#7249,#6216,.T.);
#8727=EDGE_CURVE('',#7250,#7250,#6217,.T.);
#8728=EDGE_CURVE('',#7250,#7248,#4813,.T.);
#8729=EDGE_CURVE('',#7251,#7251,#6218,.T.);
#8730=EDGE_CURVE('',#7252,#7252,#6219,.T.);
#8731=EDGE_CURVE('',#7251,#7253,#4814,.T.);
#8732=EDGE_CURVE('',#7253,#7253,#6220,.T.);
#8733=EDGE_CURVE('',#7254,#7254,#6221,.T.);
#8734=EDGE_CURVE('',#7254,#7252,#4815,.T.);
#8735=EDGE_CURVE('',#7255,#7255,#6222,.T.);
#8736=EDGE_CURVE('',#7256,#7256,#6223,.T.);
#8737=EDGE_CURVE('',#7255,#7257,#4816,.T.);
#8738=EDGE_CURVE('',#7257,#7257,#6224,.T.);
#8739=EDGE_CURVE('',#7258,#7258,#6225,.T.);
#8740=EDGE_CURVE('',#7258,#7256,#4817,.T.);
#8741=EDGE_CURVE('',#7259,#7259,#6226,.T.);
#8742=EDGE_CURVE('',#7260,#7260,#6227,.T.);
#8743=EDGE_CURVE('',#7259,#7261,#4818,.T.);
#8744=EDGE_CURVE('',#7261,#7261,#6228,.T.);
#8745=EDGE_CURVE('',#7262,#7262,#6229,.T.);
#8746=EDGE_CURVE('',#7262,#7260,#4819,.T.);
#8747=EDGE_CURVE('',#7263,#7263,#6230,.T.);
#8748=EDGE_CURVE('',#7263,#7264,#4820,.T.);
#8749=EDGE_CURVE('',#7264,#7264,#6231,.T.);
#8750=EDGE_CURVE('',#7265,#7265,#6232,.T.);
#8751=EDGE_CURVE('',#7265,#7266,#4821,.T.);
#8752=EDGE_CURVE('',#7266,#7266,#6233,.T.);
#8753=EDGE_CURVE('',#7267,#7267,#6234,.T.);
#8754=EDGE_CURVE('',#7267,#7268,#4822,.T.);
#8755=EDGE_CURVE('',#7268,#7268,#6235,.T.);
#8756=EDGE_CURVE('',#7269,#7269,#6236,.T.);
#8757=EDGE_CURVE('',#7269,#7270,#4823,.T.);
#8758=EDGE_CURVE('',#7270,#7270,#6237,.T.);
#8759=EDGE_CURVE('',#7271,#7271,#6238,.T.);
#8760=EDGE_CURVE('',#7271,#7272,#4824,.T.);
#8761=EDGE_CURVE('',#7272,#7272,#6239,.T.);
#8762=EDGE_CURVE('',#7273,#7273,#6240,.T.);
#8763=EDGE_CURVE('',#7273,#7274,#4825,.T.);
#8764=EDGE_CURVE('',#7274,#7274,#6241,.T.);
#8765=EDGE_CURVE('',#7275,#7275,#6242,.T.);
#8766=EDGE_CURVE('',#7276,#7276,#6243,.T.);
#8767=EDGE_CURVE('',#7277,#7277,#6244,.T.);
#8768=EDGE_CURVE('',#7277,#7275,#4826,.T.);
#8769=EDGE_CURVE('',#7276,#7278,#4827,.T.);
#8770=EDGE_CURVE('',#7278,#7278,#6245,.T.);
#8771=EDGE_CURVE('',#7279,#7279,#6246,.T.);
#8772=EDGE_CURVE('',#7280,#7280,#6247,.T.);
#8773=EDGE_CURVE('',#7281,#7281,#6248,.T.);
#8774=EDGE_CURVE('',#7281,#7279,#4828,.T.);
#8775=EDGE_CURVE('',#7280,#7282,#4829,.T.);
#8776=EDGE_CURVE('',#7282,#7282,#6249,.T.);
#8777=EDGE_CURVE('',#7283,#7283,#6250,.T.);
#8778=EDGE_CURVE('',#7284,#7284,#6251,.T.);
#8779=EDGE_CURVE('',#7285,#7285,#6252,.T.);
#8780=EDGE_CURVE('',#7285,#7283,#4830,.T.);
#8781=EDGE_CURVE('',#7284,#7286,#4831,.T.);
#8782=EDGE_CURVE('',#7286,#7286,#6253,.T.);
#8783=EDGE_CURVE('',#7287,#7287,#6254,.T.);
#8784=EDGE_CURVE('',#7288,#7288,#6255,.T.);
#8785=EDGE_CURVE('',#7289,#7289,#6256,.T.);
#8786=EDGE_CURVE('',#7289,#7287,#4832,.T.);
#8787=EDGE_CURVE('',#7288,#7290,#4833,.T.);
#8788=EDGE_CURVE('',#7290,#7290,#6257,.T.);
#8789=EDGE_CURVE('',#7291,#7292,#6258,.T.);
#8790=EDGE_CURVE('',#7292,#7291,#6259,.T.);
#8791=EDGE_CURVE('',#7292,#7293,#6260,.T.);
#8792=EDGE_CURVE('',#7294,#7293,#6261,.T.);
#8793=EDGE_CURVE('',#7293,#7294,#6262,.T.);
#8794=EDGE_CURVE('',#7294,#7295,#4834,.T.);
#8795=EDGE_CURVE('',#7295,#7295,#6263,.T.);
#8796=EDGE_CURVE('',#7296,#7296,#6264,.T.);
#8797=EDGE_CURVE('',#7296,#7297,#4835,.T.);
#8798=EDGE_CURVE('',#7297,#7297,#6265,.T.);
#8799=EDGE_CURVE('',#7297,#7298,#4836,.T.);
#8800=EDGE_CURVE('',#7298,#7298,#6266,.T.);
#8801=EDGE_CURVE('',#7299,#7299,#6267,.T.);
#8802=EDGE_CURVE('',#7299,#7291,#4837,.T.);
#8803=EDGE_CURVE('',#7300,#7300,#6268,.T.);
#8804=EDGE_CURVE('',#7300,#7296,#4838,.T.);
#8805=EDGE_CURVE('',#7301,#7302,#6269,.T.);
#8806=EDGE_CURVE('',#7302,#7301,#6270,.T.);
#8807=EDGE_CURVE('',#7302,#7303,#6271,.T.);
#8808=EDGE_CURVE('',#7304,#7303,#6272,.T.);
#8809=EDGE_CURVE('',#7303,#7304,#6273,.T.);
#8810=EDGE_CURVE('',#7305,#7305,#6274,.T.);
#8811=EDGE_CURVE('',#7305,#7304,#4839,.T.);
#8812=EDGE_CURVE('',#7306,#7306,#6275,.T.);
#8813=EDGE_CURVE('',#7307,#7307,#6276,.T.);
#8814=EDGE_CURVE('',#7308,#7308,#6277,.T.);
#8815=EDGE_CURVE('',#7308,#7306,#4840,.T.);
#8816=EDGE_CURVE('',#7309,#7309,#6278,.T.);
#8817=EDGE_CURVE('',#7309,#7308,#4841,.T.);
#8818=EDGE_CURVE('',#7310,#7310,#6279,.T.);
#8819=EDGE_CURVE('',#7310,#7309,#4842,.T.);
#8820=EDGE_CURVE('',#7301,#7307,#4843,.T.);
#8821=EDGE_CURVE('',#7311,#7312,#6280,.T.);
#8822=EDGE_CURVE('',#7313,#7314,#6281,.T.);
#8823=EDGE_CURVE('',#7315,#7316,#6282,.T.);
#8824=EDGE_CURVE('',#7317,#7318,#6283,.T.);
#8825=EDGE_CURVE('',#7319,#7320,#6284,.T.);
#8826=EDGE_CURVE('',#7321,#7322,#6285,.T.);
#8827=EDGE_CURVE('',#7323,#7324,#6286,.T.);
#8828=EDGE_CURVE('',#7325,#7326,#701,.T.);
#8829=EDGE_CURVE('',#7327,#7325,#6287,.T.);
#8830=EDGE_CURVE('',#7328,#7327,#702,.T.);
#8831=EDGE_CURVE('',#7326,#7328,#6288,.T.);
#8832=EDGE_CURVE('',#7328,#7329,#6289,.T.);
#8833=EDGE_CURVE('',#7329,#7330,#6290,.T.);
#8834=EDGE_CURVE('',#7326,#7330,#6291,.T.);
#8835=EDGE_CURVE('',#7327,#7331,#6292,.T.);
#8836=EDGE_CURVE('',#7331,#7329,#703,.T.);
#8837=EDGE_CURVE('',#7325,#7332,#6293,.T.);
#8838=EDGE_CURVE('',#7332,#7331,#6294,.T.);
#8839=EDGE_CURVE('',#7330,#7332,#704,.T.);
#8840=EDGE_CURVE('',#7333,#7334,#6295,.T.);
#8841=EDGE_CURVE('',#7335,#7333,#705,.T.);
#8842=EDGE_CURVE('',#7336,#7335,#6296,.T.);
#8843=EDGE_CURVE('',#7334,#7336,#706,.T.);
#8844=EDGE_CURVE('',#7335,#7337,#6297,.T.);
#8845=EDGE_CURVE('',#7337,#7338,#6298,.T.);
#8846=EDGE_CURVE('',#7336,#7338,#6299,.T.);
#8847=EDGE_CURVE('',#7338,#7339,#707,.T.);
#8848=EDGE_CURVE('',#7334,#7339,#6300,.T.);
#8849=EDGE_CURVE('',#7333,#7340,#6301,.T.);
#8850=EDGE_CURVE('',#7340,#7337,#708,.T.);
#8851=EDGE_CURVE('',#7339,#7340,#6302,.T.);
#8852=EDGE_CURVE('',#7341,#7342,#709,.T.);
#8853=EDGE_CURVE('',#7343,#7341,#6303,.T.);
#8854=EDGE_CURVE('',#7344,#7343,#710,.T.);
#8855=EDGE_CURVE('',#7342,#7344,#6304,.T.);
#8856=EDGE_CURVE('',#7343,#7345,#6305,.T.);
#8857=EDGE_CURVE('',#7345,#7346,#711,.T.);
#8858=EDGE_CURVE('',#7344,#7346,#6306,.T.);
#8859=EDGE_CURVE('',#7346,#7347,#6307,.T.);
#8860=EDGE_CURVE('',#7342,#7347,#6308,.T.);
#8861=EDGE_CURVE('',#7341,#7348,#6309,.T.);
#8862=EDGE_CURVE('',#7348,#7345,#6310,.T.);
#8863=EDGE_CURVE('',#7347,#7348,#712,.T.);
#8864=EDGE_CURVE('',#7349,#7350,#6311,.T.);
#8865=EDGE_CURVE('',#7351,#7349,#713,.T.);
#8866=EDGE_CURVE('',#7352,#7351,#6312,.T.);
#8867=EDGE_CURVE('',#7350,#7352,#714,.T.);
#8868=EDGE_CURVE('',#7353,#7352,#6313,.T.);
#8869=EDGE_CURVE('',#7353,#7354,#715,.T.);
#8870=EDGE_CURVE('',#7354,#7350,#6314,.T.);
#8871=EDGE_CURVE('',#7355,#7351,#6315,.T.);
#8872=EDGE_CURVE('',#7355,#7353,#6316,.T.);
#8873=EDGE_CURVE('',#7356,#7349,#6317,.T.);
#8874=EDGE_CURVE('',#7356,#7355,#716,.T.);
#8875=EDGE_CURVE('',#7354,#7356,#6318,.T.);
#8876=EDGE_CURVE('',#7357,#7358,#717,.T.);
#8877=EDGE_CURVE('',#7359,#7357,#6319,.T.);
#8878=EDGE_CURVE('',#7360,#7359,#718,.T.);
#8879=EDGE_CURVE('',#7358,#7360,#6320,.T.);
#8880=EDGE_CURVE('',#7361,#7362,#719,.T.);
#8881=EDGE_CURVE('',#7362,#7357,#6321,.T.);
#8882=EDGE_CURVE('',#7361,#7358,#6322,.T.);
#8883=EDGE_CURVE('',#7363,#7361,#6323,.T.);
#8884=EDGE_CURVE('',#7363,#7360,#6324,.T.);
#8885=EDGE_CURVE('',#7362,#7364,#6325,.T.);
#8886=EDGE_CURVE('',#7364,#7359,#6326,.T.);
#8887=EDGE_CURVE('',#7364,#7363,#720,.T.);
#8888=EDGE_CURVE('',#7365,#7366,#721,.T.);
#8889=EDGE_CURVE('',#7367,#7365,#6327,.T.);
#8890=EDGE_CURVE('',#7368,#7367,#722,.T.);
#8891=EDGE_CURVE('',#7366,#7368,#6328,.T.);
#8892=EDGE_CURVE('',#7369,#7370,#723,.T.);
#8893=EDGE_CURVE('',#7370,#7365,#6329,.T.);
#8894=EDGE_CURVE('',#7369,#7366,#6330,.T.);
#8895=EDGE_CURVE('',#7371,#7369,#6331,.T.);
#8896=EDGE_CURVE('',#7371,#7368,#6332,.T.);
#8897=EDGE_CURVE('',#7372,#7371,#724,.T.);
#8898=EDGE_CURVE('',#7372,#7367,#6333,.T.);
#8899=EDGE_CURVE('',#7370,#7372,#6334,.T.);
#8900=EDGE_CURVE('',#7373,#7374,#725,.T.);
#8901=EDGE_CURVE('',#7374,#7375,#6335,.T.);
#8902=EDGE_CURVE('',#7375,#7376,#726,.T.);
#8903=EDGE_CURVE('',#7373,#7376,#6336,.T.);
#8904=EDGE_CURVE('',#7377,#7373,#6337,.T.);
#8905=EDGE_CURVE('',#7376,#7378,#6338,.T.);
#8906=EDGE_CURVE('',#7377,#7378,#6339,.T.);
#8907=EDGE_CURVE('',#7379,#7375,#6340,.T.);
#8908=EDGE_CURVE('',#7378,#7379,#727,.T.);
#8909=EDGE_CURVE('',#7374,#7380,#6341,.T.);
#8910=EDGE_CURVE('',#7380,#7379,#6342,.T.);
#8911=EDGE_CURVE('',#7380,#7377,#728,.T.);
#8912=EDGE_CURVE('',#7381,#7381,#6343,.T.);
#8913=EDGE_CURVE('',#7382,#7382,#6344,.T.);
#8914=EDGE_CURVE('',#7383,#7383,#6345,.T.);
#8915=EDGE_CURVE('',#7383,#7381,#4844,.T.);
#8916=EDGE_CURVE('',#7384,#7384,#6346,.T.);
#8917=EDGE_CURVE('',#7384,#7382,#4845,.T.);
#8918=EDGE_CURVE('',#7385,#7385,#6347,.T.);
#8919=EDGE_CURVE('',#7386,#7386,#6348,.T.);
#8920=EDGE_CURVE('',#7387,#7387,#6349,.T.);
#8921=EDGE_CURVE('',#7387,#7385,#4846,.T.);
#8922=EDGE_CURVE('',#7388,#7388,#6350,.T.);
#8923=EDGE_CURVE('',#7388,#7386,#4847,.T.);
#8924=EDGE_CURVE('',#7389,#7389,#6351,.T.);
#8925=EDGE_CURVE('',#7390,#7390,#6352,.T.);
#8926=EDGE_CURVE('',#7391,#7391,#6353,.T.);
#8927=EDGE_CURVE('',#7392,#7392,#6354,.T.);
#8928=EDGE_CURVE('',#7389,#7391,#4848,.T.);
#8929=EDGE_CURVE('',#7392,#7393,#4849,.T.);
#8930=EDGE_CURVE('',#7393,#7393,#6355,.T.);
#8931=EDGE_CURVE('',#7394,#7394,#6356,.T.);
#8932=EDGE_CURVE('',#7395,#7395,#6357,.T.);
#8933=EDGE_CURVE('',#7396,#7396,#6358,.T.);
#8934=EDGE_CURVE('',#7394,#7395,#4850,.T.);
#8935=EDGE_CURVE('',#7396,#7397,#4851,.T.);
#8936=EDGE_CURVE('',#7397,#7397,#6359,.T.);
#8937=EDGE_CURVE('',#7398,#7398,#6360,.T.);
#8938=EDGE_CURVE('',#7398,#7390,#4852,.T.);
#8939=EDGE_CURVE('',#7399,#7399,#6361,.T.);
#8940=EDGE_CURVE('',#7399,#7400,#4853,.T.);
#8941=EDGE_CURVE('',#7400,#7400,#6362,.T.);
#8942=EDGE_CURVE('',#7401,#7401,#6363,.T.);
#8943=EDGE_CURVE('',#7401,#7402,#4854,.T.);
#8944=EDGE_CURVE('',#7402,#7402,#6364,.T.);
#8945=EDGE_CURVE('',#7403,#7403,#6365,.T.);
#8946=EDGE_CURVE('',#7403,#7404,#4855,.T.);
#8947=EDGE_CURVE('',#7404,#7404,#6366,.T.);
#8948=EDGE_CURVE('',#7405,#7405,#6367,.T.);
#8949=EDGE_CURVE('',#7405,#7406,#4856,.T.);
#8950=EDGE_CURVE('',#7406,#7406,#6368,.T.);
#8951=EDGE_CURVE('',#7407,#7407,#6369,.T.);
#8952=EDGE_CURVE('',#7407,#7408,#4857,.T.);
#8953=EDGE_CURVE('',#7408,#7408,#6370,.T.);
#8954=EDGE_CURVE('',#7409,#7409,#6371,.T.);
#8955=EDGE_CURVE('',#7409,#7410,#4858,.T.);
#8956=EDGE_CURVE('',#7410,#7410,#6372,.T.);
#8957=EDGE_CURVE('',#7411,#7411,#6373,.T.);
#8958=EDGE_CURVE('',#7411,#7412,#4859,.T.);
#8959=EDGE_CURVE('',#7412,#7412,#6374,.T.);
#8960=EDGE_CURVE('',#7413,#7413,#6375,.T.);
#8961=EDGE_CURVE('',#7413,#7414,#4860,.T.);
#8962=EDGE_CURVE('',#7414,#7414,#6376,.T.);
#8963=EDGE_CURVE('',#7415,#7415,#6377,.T.);
#8964=EDGE_CURVE('',#7415,#7416,#4861,.T.);
#8965=EDGE_CURVE('',#7416,#7416,#6378,.T.);
#8966=EDGE_CURVE('',#7417,#7417,#6379,.T.);
#8967=EDGE_CURVE('',#7417,#7418,#4862,.T.);
#8968=EDGE_CURVE('',#7418,#7418,#6380,.T.);
#8969=EDGE_CURVE('',#7419,#7419,#6381,.T.);
#8970=EDGE_CURVE('',#7419,#7420,#4863,.T.);
#8971=EDGE_CURVE('',#7420,#7420,#6382,.T.);
#8972=ORIENTED_EDGE('',*,*,#7421,.F.);
#8973=ORIENTED_EDGE('',*,*,#7422,.T.);
#8974=ORIENTED_EDGE('',*,*,#7423,.F.);
#8975=ORIENTED_EDGE('',*,*,#7422,.F.);
#8976=ORIENTED_EDGE('',*,*,#7424,.F.);
#8977=ORIENTED_EDGE('',*,*,#7425,.T.);
#8978=ORIENTED_EDGE('',*,*,#7426,.F.);
#8979=ORIENTED_EDGE('',*,*,#7425,.F.);
#8980=ORIENTED_EDGE('',*,*,#7427,.F.);
#8981=ORIENTED_EDGE('',*,*,#7428,.T.);
#8982=ORIENTED_EDGE('',*,*,#7429,.F.);
#8983=ORIENTED_EDGE('',*,*,#7428,.F.);
#8984=ORIENTED_EDGE('',*,*,#7430,.F.);
#8985=ORIENTED_EDGE('',*,*,#7431,.T.);
#8986=ORIENTED_EDGE('',*,*,#7432,.F.);
#8987=ORIENTED_EDGE('',*,*,#7431,.F.);
#8988=ORIENTED_EDGE('',*,*,#7433,.F.);
#8989=ORIENTED_EDGE('',*,*,#7434,.T.);
#8990=ORIENTED_EDGE('',*,*,#7435,.F.);
#8991=ORIENTED_EDGE('',*,*,#7434,.F.);
#8992=ORIENTED_EDGE('',*,*,#7436,.F.);
#8993=ORIENTED_EDGE('',*,*,#7437,.T.);
#8994=ORIENTED_EDGE('',*,*,#7438,.F.);
#8995=ORIENTED_EDGE('',*,*,#7437,.F.);
#8996=ORIENTED_EDGE('',*,*,#7439,.F.);
#8997=ORIENTED_EDGE('',*,*,#7440,.T.);
#8998=ORIENTED_EDGE('',*,*,#7441,.F.);
#8999=ORIENTED_EDGE('',*,*,#7440,.F.);
#9000=ORIENTED_EDGE('',*,*,#7442,.F.);
#9001=ORIENTED_EDGE('',*,*,#7443,.T.);
#9002=ORIENTED_EDGE('',*,*,#7444,.F.);
#9003=ORIENTED_EDGE('',*,*,#7443,.F.);
#9004=ORIENTED_EDGE('',*,*,#7445,.T.);
#9005=ORIENTED_EDGE('',*,*,#7446,.T.);
#9006=ORIENTED_EDGE('',*,*,#7447,.F.);
#9007=ORIENTED_EDGE('',*,*,#7448,.F.);
#9008=ORIENTED_EDGE('',*,*,#7449,.T.);
#9009=ORIENTED_EDGE('',*,*,#7448,.T.);
#9010=ORIENTED_EDGE('',*,*,#7450,.F.);
#9011=ORIENTED_EDGE('',*,*,#7451,.F.);
#9012=ORIENTED_EDGE('',*,*,#7452,.T.);
#9013=ORIENTED_EDGE('',*,*,#7451,.T.);
#9014=ORIENTED_EDGE('',*,*,#7453,.F.);
#9015=ORIENTED_EDGE('',*,*,#7454,.F.);
#9016=ORIENTED_EDGE('',*,*,#7455,.T.);
#9017=ORIENTED_EDGE('',*,*,#7454,.T.);
#9018=ORIENTED_EDGE('',*,*,#7456,.F.);
#9019=ORIENTED_EDGE('',*,*,#7446,.F.);
#9020=ORIENTED_EDGE('',*,*,#7456,.T.);
#9021=ORIENTED_EDGE('',*,*,#7453,.T.);
#9022=ORIENTED_EDGE('',*,*,#7450,.T.);
#9023=ORIENTED_EDGE('',*,*,#7447,.T.);
#9024=ORIENTED_EDGE('',*,*,#7444,.T.);
#9025=ORIENTED_EDGE('',*,*,#7441,.T.);
#9026=ORIENTED_EDGE('',*,*,#7438,.T.);
#9027=ORIENTED_EDGE('',*,*,#7435,.T.);
#9028=ORIENTED_EDGE('',*,*,#7432,.T.);
#9029=ORIENTED_EDGE('',*,*,#7429,.T.);
#9030=ORIENTED_EDGE('',*,*,#7426,.T.);
#9031=ORIENTED_EDGE('',*,*,#7423,.T.);
#9032=ORIENTED_EDGE('',*,*,#7455,.F.);
#9033=ORIENTED_EDGE('',*,*,#7445,.F.);
#9034=ORIENTED_EDGE('',*,*,#7449,.F.);
#9035=ORIENTED_EDGE('',*,*,#7452,.F.);
#9036=ORIENTED_EDGE('',*,*,#7442,.T.);
#9037=ORIENTED_EDGE('',*,*,#7439,.T.);
#9038=ORIENTED_EDGE('',*,*,#7436,.T.);
#9039=ORIENTED_EDGE('',*,*,#7433,.T.);
#9040=ORIENTED_EDGE('',*,*,#7430,.T.);
#9041=ORIENTED_EDGE('',*,*,#7427,.T.);
#9042=ORIENTED_EDGE('',*,*,#7424,.T.);
#9043=ORIENTED_EDGE('',*,*,#7421,.T.);
#9044=ORIENTED_EDGE('',*,*,#7457,.T.);
#9045=ORIENTED_EDGE('',*,*,#7458,.T.);
#9046=ORIENTED_EDGE('',*,*,#7459,.F.);
#9047=ORIENTED_EDGE('',*,*,#7460,.F.);
#9048=ORIENTED_EDGE('',*,*,#7461,.T.);
#9049=ORIENTED_EDGE('',*,*,#7460,.T.);
#9050=ORIENTED_EDGE('',*,*,#7462,.F.);
#9051=ORIENTED_EDGE('',*,*,#7463,.F.);
#9052=ORIENTED_EDGE('',*,*,#7464,.T.);
#9053=ORIENTED_EDGE('',*,*,#7463,.T.);
#9054=ORIENTED_EDGE('',*,*,#7465,.F.);
#9055=ORIENTED_EDGE('',*,*,#7466,.F.);
#9056=ORIENTED_EDGE('',*,*,#7467,.T.);
#9057=ORIENTED_EDGE('',*,*,#7466,.T.);
#9058=ORIENTED_EDGE('',*,*,#7468,.F.);
#9059=ORIENTED_EDGE('',*,*,#7458,.F.);
#9060=ORIENTED_EDGE('',*,*,#7468,.T.);
#9061=ORIENTED_EDGE('',*,*,#7465,.T.);
#9062=ORIENTED_EDGE('',*,*,#7462,.T.);
#9063=ORIENTED_EDGE('',*,*,#7459,.T.);
#9064=ORIENTED_EDGE('',*,*,#7467,.F.);
#9065=ORIENTED_EDGE('',*,*,#7457,.F.);
#9066=ORIENTED_EDGE('',*,*,#7461,.F.);
#9067=ORIENTED_EDGE('',*,*,#7464,.F.);
#9068=ORIENTED_EDGE('',*,*,#7469,.T.);
#9069=ORIENTED_EDGE('',*,*,#7470,.T.);
#9070=ORIENTED_EDGE('',*,*,#7471,.F.);
#9071=ORIENTED_EDGE('',*,*,#7472,.F.);
#9072=ORIENTED_EDGE('',*,*,#7473,.T.);
#9073=ORIENTED_EDGE('',*,*,#7472,.T.);
#9074=ORIENTED_EDGE('',*,*,#7474,.F.);
#9075=ORIENTED_EDGE('',*,*,#7475,.F.);
#9076=ORIENTED_EDGE('',*,*,#7476,.T.);
#9077=ORIENTED_EDGE('',*,*,#7475,.T.);
#9078=ORIENTED_EDGE('',*,*,#7477,.F.);
#9079=ORIENTED_EDGE('',*,*,#7478,.F.);
#9080=ORIENTED_EDGE('',*,*,#7479,.T.);
#9081=ORIENTED_EDGE('',*,*,#7478,.T.);
#9082=ORIENTED_EDGE('',*,*,#7480,.F.);
#9083=ORIENTED_EDGE('',*,*,#7470,.F.);
#9084=ORIENTED_EDGE('',*,*,#7480,.T.);
#9085=ORIENTED_EDGE('',*,*,#7477,.T.);
#9086=ORIENTED_EDGE('',*,*,#7474,.T.);
#9087=ORIENTED_EDGE('',*,*,#7471,.T.);
#9088=ORIENTED_EDGE('',*,*,#7479,.F.);
#9089=ORIENTED_EDGE('',*,*,#7469,.F.);
#9090=ORIENTED_EDGE('',*,*,#7473,.F.);
#9091=ORIENTED_EDGE('',*,*,#7476,.F.);
#9092=ORIENTED_EDGE('',*,*,#7481,.F.);
#9093=ORIENTED_EDGE('',*,*,#7482,.T.);
#9094=ORIENTED_EDGE('',*,*,#7483,.F.);
#9095=ORIENTED_EDGE('',*,*,#7482,.F.);
#9096=ORIENTED_EDGE('',*,*,#7484,.F.);
#9097=ORIENTED_EDGE('',*,*,#7485,.T.);
#9098=ORIENTED_EDGE('',*,*,#7486,.F.);
#9099=ORIENTED_EDGE('',*,*,#7485,.F.);
#9100=ORIENTED_EDGE('',*,*,#7487,.F.);
#9101=ORIENTED_EDGE('',*,*,#7488,.T.);
#9102=ORIENTED_EDGE('',*,*,#7489,.F.);
#9103=ORIENTED_EDGE('',*,*,#7488,.F.);
#9104=ORIENTED_EDGE('',*,*,#7490,.F.);
#9105=ORIENTED_EDGE('',*,*,#7491,.T.);
#9106=ORIENTED_EDGE('',*,*,#7492,.F.);
#9107=ORIENTED_EDGE('',*,*,#7491,.F.);
#9108=ORIENTED_EDGE('',*,*,#7493,.F.);
#9109=ORIENTED_EDGE('',*,*,#7494,.T.);
#9110=ORIENTED_EDGE('',*,*,#7495,.F.);
#9111=ORIENTED_EDGE('',*,*,#7494,.F.);
#9112=ORIENTED_EDGE('',*,*,#7496,.F.);
#9113=ORIENTED_EDGE('',*,*,#7497,.T.);
#9114=ORIENTED_EDGE('',*,*,#7498,.F.);
#9115=ORIENTED_EDGE('',*,*,#7497,.F.);
#9116=ORIENTED_EDGE('',*,*,#7499,.F.);
#9117=ORIENTED_EDGE('',*,*,#7500,.T.);
#9118=ORIENTED_EDGE('',*,*,#7501,.F.);
#9119=ORIENTED_EDGE('',*,*,#7500,.F.);
#9120=ORIENTED_EDGE('',*,*,#7502,.F.);
#9121=ORIENTED_EDGE('',*,*,#7503,.T.);
#9122=ORIENTED_EDGE('',*,*,#7504,.F.);
#9123=ORIENTED_EDGE('',*,*,#7503,.F.);
#9124=ORIENTED_EDGE('',*,*,#7505,.F.);
#9125=ORIENTED_EDGE('',*,*,#7506,.T.);
#9126=ORIENTED_EDGE('',*,*,#7507,.F.);
#9127=ORIENTED_EDGE('',*,*,#7506,.F.);
#9128=ORIENTED_EDGE('',*,*,#7508,.F.);
#9129=ORIENTED_EDGE('',*,*,#7509,.T.);
#9130=ORIENTED_EDGE('',*,*,#7510,.T.);
#9131=ORIENTED_EDGE('',*,*,#7511,.T.);
#9132=ORIENTED_EDGE('',*,*,#7501,.T.);
#9133=ORIENTED_EDGE('',*,*,#7504,.T.);
#9134=ORIENTED_EDGE('',*,*,#7512,.F.);
#9135=ORIENTED_EDGE('',*,*,#7513,.T.);
#9136=ORIENTED_EDGE('',*,*,#7514,.T.);
#9137=ORIENTED_EDGE('',*,*,#7515,.T.);
#9138=ORIENTED_EDGE('',*,*,#7498,.T.);
#9139=ORIENTED_EDGE('',*,*,#7507,.T.);
#9140=ORIENTED_EDGE('',*,*,#7516,.T.);
#9141=ORIENTED_EDGE('',*,*,#7517,.T.);
#9142=ORIENTED_EDGE('',*,*,#7514,.F.);
#9143=ORIENTED_EDGE('',*,*,#7518,.F.);
#9144=ORIENTED_EDGE('',*,*,#7519,.T.);
#9145=ORIENTED_EDGE('',*,*,#7520,.T.);
#9146=ORIENTED_EDGE('',*,*,#7510,.F.);
#9147=ORIENTED_EDGE('',*,*,#7521,.F.);
#9148=ORIENTED_EDGE('',*,*,#7522,.T.);
#9149=ORIENTED_EDGE('',*,*,#7523,.F.);
#9150=ORIENTED_EDGE('',*,*,#7524,.F.);
#9151=ORIENTED_EDGE('',*,*,#7515,.F.);
#9152=ORIENTED_EDGE('',*,*,#7517,.F.);
#9153=ORIENTED_EDGE('',*,*,#7525,.T.);
#9154=ORIENTED_EDGE('',*,*,#7521,.T.);
#9155=ORIENTED_EDGE('',*,*,#7509,.F.);
#9156=ORIENTED_EDGE('',*,*,#7526,.T.);
#9157=ORIENTED_EDGE('',*,*,#7508,.T.);
#9158=ORIENTED_EDGE('',*,*,#7527,.T.);
#9159=ORIENTED_EDGE('',*,*,#7528,.F.);
#9160=ORIENTED_EDGE('',*,*,#7522,.F.);
#9161=ORIENTED_EDGE('',*,*,#7529,.T.);
#9162=ORIENTED_EDGE('',*,*,#7530,.T.);
#9163=ORIENTED_EDGE('',*,*,#7493,.T.);
#9164=ORIENTED_EDGE('',*,*,#7490,.T.);
#9165=ORIENTED_EDGE('',*,*,#7487,.T.);
#9166=ORIENTED_EDGE('',*,*,#7484,.T.);
#9167=ORIENTED_EDGE('',*,*,#7481,.T.);
#9168=ORIENTED_EDGE('',*,*,#7531,.F.);
#9169=ORIENTED_EDGE('',*,*,#7532,.T.);
#9170=ORIENTED_EDGE('',*,*,#7526,.F.);
#9171=ORIENTED_EDGE('',*,*,#7532,.F.);
#9172=ORIENTED_EDGE('',*,*,#7529,.F.);
#9173=ORIENTED_EDGE('',*,*,#7533,.T.);
#9174=ORIENTED_EDGE('',*,*,#7534,.F.);
#9175=ORIENTED_EDGE('',*,*,#7533,.F.);
#9176=ORIENTED_EDGE('',*,*,#7530,.F.);
#9177=ORIENTED_EDGE('',*,*,#7535,.T.);
#9178=ORIENTED_EDGE('',*,*,#7536,.F.);
#9179=ORIENTED_EDGE('',*,*,#7535,.F.);
#9180=ORIENTED_EDGE('',*,*,#7512,.T.);
#9181=ORIENTED_EDGE('',*,*,#7524,.T.);
#9182=ORIENTED_EDGE('',*,*,#7537,.F.);
#9183=ORIENTED_EDGE('',*,*,#7538,.F.);
#9184=ORIENTED_EDGE('',*,*,#7536,.T.);
#9185=ORIENTED_EDGE('',*,*,#7534,.T.);
#9186=ORIENTED_EDGE('',*,*,#7495,.T.);
#9187=ORIENTED_EDGE('',*,*,#7492,.T.);
#9188=ORIENTED_EDGE('',*,*,#7489,.T.);
#9189=ORIENTED_EDGE('',*,*,#7486,.T.);
#9190=ORIENTED_EDGE('',*,*,#7483,.T.);
#9191=ORIENTED_EDGE('',*,*,#7538,.T.);
#9192=ORIENTED_EDGE('',*,*,#7539,.F.);
#9193=ORIENTED_EDGE('',*,*,#7527,.F.);
#9194=ORIENTED_EDGE('',*,*,#7511,.F.);
#9195=ORIENTED_EDGE('',*,*,#7520,.F.);
#9196=ORIENTED_EDGE('',*,*,#7540,.T.);
#9197=ORIENTED_EDGE('',*,*,#7518,.T.);
#9198=ORIENTED_EDGE('',*,*,#7513,.F.);
#9199=ORIENTED_EDGE('',*,*,#7531,.T.);
#9200=ORIENTED_EDGE('',*,*,#7528,.T.);
#9201=ORIENTED_EDGE('',*,*,#7539,.T.);
#9202=ORIENTED_EDGE('',*,*,#7537,.T.);
#9203=ORIENTED_EDGE('',*,*,#7523,.T.);
#9204=ORIENTED_EDGE('',*,*,#7525,.F.);
#9205=ORIENTED_EDGE('',*,*,#7516,.F.);
#9206=ORIENTED_EDGE('',*,*,#7540,.F.);
#9207=ORIENTED_EDGE('',*,*,#7519,.F.);
#9208=ORIENTED_EDGE('',*,*,#7496,.T.);
#9209=ORIENTED_EDGE('',*,*,#7499,.T.);
#9210=ORIENTED_EDGE('',*,*,#7502,.T.);
#9211=ORIENTED_EDGE('',*,*,#7505,.T.);
#9212=ORIENTED_EDGE('',*,*,#7541,.F.);
#9213=ORIENTED_EDGE('',*,*,#7542,.T.);
#9214=ORIENTED_EDGE('',*,*,#7543,.F.);
#9215=ORIENTED_EDGE('',*,*,#7542,.F.);
#9216=ORIENTED_EDGE('',*,*,#7544,.F.);
#9217=ORIENTED_EDGE('',*,*,#7545,.T.);
#9218=ORIENTED_EDGE('',*,*,#7546,.F.);
#9219=ORIENTED_EDGE('',*,*,#7545,.F.);
#9220=ORIENTED_EDGE('',*,*,#7547,.F.);
#9221=ORIENTED_EDGE('',*,*,#7548,.T.);
#9222=ORIENTED_EDGE('',*,*,#7549,.F.);
#9223=ORIENTED_EDGE('',*,*,#7548,.F.);
#9224=ORIENTED_EDGE('',*,*,#7550,.F.);
#9225=ORIENTED_EDGE('',*,*,#7551,.T.);
#9226=ORIENTED_EDGE('',*,*,#7552,.F.);
#9227=ORIENTED_EDGE('',*,*,#7551,.F.);
#9228=ORIENTED_EDGE('',*,*,#7553,.F.);
#9229=ORIENTED_EDGE('',*,*,#7554,.T.);
#9230=ORIENTED_EDGE('',*,*,#7555,.F.);
#9231=ORIENTED_EDGE('',*,*,#7554,.F.);
#9232=ORIENTED_EDGE('',*,*,#7553,.T.);
#9233=ORIENTED_EDGE('',*,*,#7556,.T.);
#9234=ORIENTED_EDGE('',*,*,#7556,.F.);
#9235=ORIENTED_EDGE('',*,*,#7557,.T.);
#9236=ORIENTED_EDGE('',*,*,#7558,.T.);
#9237=ORIENTED_EDGE('',*,*,#7557,.F.);
#9238=ORIENTED_EDGE('',*,*,#7559,.F.);
#9239=ORIENTED_EDGE('',*,*,#7560,.T.);
#9240=ORIENTED_EDGE('',*,*,#7561,.T.);
#9241=ORIENTED_EDGE('',*,*,#7560,.F.);
#9242=ORIENTED_EDGE('',*,*,#7559,.T.);
#9243=ORIENTED_EDGE('',*,*,#7555,.T.);
#9244=ORIENTED_EDGE('',*,*,#7552,.T.);
#9245=ORIENTED_EDGE('',*,*,#7549,.T.);
#9246=ORIENTED_EDGE('',*,*,#7546,.T.);
#9247=ORIENTED_EDGE('',*,*,#7543,.T.);
#9248=ORIENTED_EDGE('',*,*,#7561,.F.);
#9249=ORIENTED_EDGE('',*,*,#7558,.F.);
#9250=ORIENTED_EDGE('',*,*,#7550,.T.);
#9251=ORIENTED_EDGE('',*,*,#7547,.T.);
#9252=ORIENTED_EDGE('',*,*,#7544,.T.);
#9253=ORIENTED_EDGE('',*,*,#7541,.T.);
#9254=ORIENTED_EDGE('',*,*,#7562,.F.);
#9255=ORIENTED_EDGE('',*,*,#7563,.T.);
#9256=ORIENTED_EDGE('',*,*,#7564,.F.);
#9257=ORIENTED_EDGE('',*,*,#7563,.F.);
#9258=ORIENTED_EDGE('',*,*,#7565,.F.);
#9259=ORIENTED_EDGE('',*,*,#7566,.T.);
#9260=ORIENTED_EDGE('',*,*,#7567,.F.);
#9261=ORIENTED_EDGE('',*,*,#7566,.F.);
#9262=ORIENTED_EDGE('',*,*,#7568,.F.);
#9263=ORIENTED_EDGE('',*,*,#7569,.T.);
#9264=ORIENTED_EDGE('',*,*,#7570,.F.);
#9265=ORIENTED_EDGE('',*,*,#7569,.F.);
#9266=ORIENTED_EDGE('',*,*,#7571,.F.);
#9267=ORIENTED_EDGE('',*,*,#7572,.T.);
#9268=ORIENTED_EDGE('',*,*,#7573,.F.);
#9269=ORIENTED_EDGE('',*,*,#7572,.F.);
#9270=ORIENTED_EDGE('',*,*,#7574,.F.);
#9271=ORIENTED_EDGE('',*,*,#7575,.T.);
#9272=ORIENTED_EDGE('',*,*,#7576,.T.);
#9273=ORIENTED_EDGE('',*,*,#7575,.F.);
#9274=ORIENTED_EDGE('',*,*,#7576,.F.);
#9275=ORIENTED_EDGE('',*,*,#7577,.F.);
#9276=ORIENTED_EDGE('',*,*,#7578,.F.);
#9277=ORIENTED_EDGE('',*,*,#7579,.T.);
#9278=ORIENTED_EDGE('',*,*,#7577,.T.);
#9279=ORIENTED_EDGE('',*,*,#7579,.F.);
#9280=ORIENTED_EDGE('',*,*,#7580,.F.);
#9281=ORIENTED_EDGE('',*,*,#7581,.T.);
#9282=ORIENTED_EDGE('',*,*,#7582,.T.);
#9283=ORIENTED_EDGE('',*,*,#7581,.F.);
#9284=ORIENTED_EDGE('',*,*,#7580,.T.);
#9285=ORIENTED_EDGE('',*,*,#7578,.T.);
#9286=ORIENTED_EDGE('',*,*,#7573,.T.);
#9287=ORIENTED_EDGE('',*,*,#7570,.T.);
#9288=ORIENTED_EDGE('',*,*,#7567,.T.);
#9289=ORIENTED_EDGE('',*,*,#7564,.T.);
#9290=ORIENTED_EDGE('',*,*,#7582,.F.);
#9291=ORIENTED_EDGE('',*,*,#7574,.T.);
#9292=ORIENTED_EDGE('',*,*,#7571,.T.);
#9293=ORIENTED_EDGE('',*,*,#7568,.T.);
#9294=ORIENTED_EDGE('',*,*,#7565,.T.);
#9295=ORIENTED_EDGE('',*,*,#7562,.T.);
#9296=ORIENTED_EDGE('',*,*,#7583,.F.);
#9297=ORIENTED_EDGE('',*,*,#7584,.T.);
#9298=ORIENTED_EDGE('',*,*,#7585,.F.);
#9299=ORIENTED_EDGE('',*,*,#7584,.F.);
#9300=ORIENTED_EDGE('',*,*,#7586,.F.);
#9301=ORIENTED_EDGE('',*,*,#7587,.T.);
#9302=ORIENTED_EDGE('',*,*,#7588,.F.);
#9303=ORIENTED_EDGE('',*,*,#7587,.F.);
#9304=ORIENTED_EDGE('',*,*,#7589,.F.);
#9305=ORIENTED_EDGE('',*,*,#7590,.T.);
#9306=ORIENTED_EDGE('',*,*,#7591,.F.);
#9307=ORIENTED_EDGE('',*,*,#7590,.F.);
#9308=ORIENTED_EDGE('',*,*,#7592,.F.);
#9309=ORIENTED_EDGE('',*,*,#7593,.T.);
#9310=ORIENTED_EDGE('',*,*,#7594,.F.);
#9311=ORIENTED_EDGE('',*,*,#7593,.F.);
#9312=ORIENTED_EDGE('',*,*,#7595,.F.);
#9313=ORIENTED_EDGE('',*,*,#7596,.T.);
#9314=ORIENTED_EDGE('',*,*,#7597,.F.);
#9315=ORIENTED_EDGE('',*,*,#7596,.F.);
#9316=ORIENTED_EDGE('',*,*,#7598,.F.);
#9317=ORIENTED_EDGE('',*,*,#7599,.T.);
#9318=ORIENTED_EDGE('',*,*,#7600,.F.);
#9319=ORIENTED_EDGE('',*,*,#7599,.F.);
#9320=ORIENTED_EDGE('',*,*,#7601,.F.);
#9321=ORIENTED_EDGE('',*,*,#7602,.T.);
#9322=ORIENTED_EDGE('',*,*,#7603,.F.);
#9323=ORIENTED_EDGE('',*,*,#7602,.F.);
#9324=ORIENTED_EDGE('',*,*,#7604,.F.);
#9325=ORIENTED_EDGE('',*,*,#7605,.T.);
#9326=ORIENTED_EDGE('',*,*,#7606,.F.);
#9327=ORIENTED_EDGE('',*,*,#7605,.F.);
#9328=ORIENTED_EDGE('',*,*,#7607,.F.);
#9329=ORIENTED_EDGE('',*,*,#7608,.T.);
#9330=ORIENTED_EDGE('',*,*,#7609,.F.);
#9331=ORIENTED_EDGE('',*,*,#7608,.F.);
#9332=ORIENTED_EDGE('',*,*,#7610,.F.);
#9333=ORIENTED_EDGE('',*,*,#7611,.T.);
#9334=ORIENTED_EDGE('',*,*,#7612,.T.);
#9335=ORIENTED_EDGE('',*,*,#7613,.T.);
#9336=ORIENTED_EDGE('',*,*,#7603,.T.);
#9337=ORIENTED_EDGE('',*,*,#7606,.T.);
#9338=ORIENTED_EDGE('',*,*,#7614,.F.);
#9339=ORIENTED_EDGE('',*,*,#7615,.T.);
#9340=ORIENTED_EDGE('',*,*,#7616,.T.);
#9341=ORIENTED_EDGE('',*,*,#7617,.T.);
#9342=ORIENTED_EDGE('',*,*,#7600,.T.);
#9343=ORIENTED_EDGE('',*,*,#7609,.T.);
#9344=ORIENTED_EDGE('',*,*,#7618,.T.);
#9345=ORIENTED_EDGE('',*,*,#7619,.T.);
#9346=ORIENTED_EDGE('',*,*,#7616,.F.);
#9347=ORIENTED_EDGE('',*,*,#7620,.F.);
#9348=ORIENTED_EDGE('',*,*,#7621,.T.);
#9349=ORIENTED_EDGE('',*,*,#7622,.T.);
#9350=ORIENTED_EDGE('',*,*,#7612,.F.);
#9351=ORIENTED_EDGE('',*,*,#7623,.F.);
#9352=ORIENTED_EDGE('',*,*,#7624,.T.);
#9353=ORIENTED_EDGE('',*,*,#7625,.F.);
#9354=ORIENTED_EDGE('',*,*,#7626,.F.);
#9355=ORIENTED_EDGE('',*,*,#7617,.F.);
#9356=ORIENTED_EDGE('',*,*,#7619,.F.);
#9357=ORIENTED_EDGE('',*,*,#7627,.T.);
#9358=ORIENTED_EDGE('',*,*,#7623,.T.);
#9359=ORIENTED_EDGE('',*,*,#7611,.F.);
#9360=ORIENTED_EDGE('',*,*,#7610,.T.);
#9361=ORIENTED_EDGE('',*,*,#7628,.T.);
#9362=ORIENTED_EDGE('',*,*,#7629,.F.);
#9363=ORIENTED_EDGE('',*,*,#7624,.F.);
#9364=ORIENTED_EDGE('',*,*,#7630,.T.);
#9365=ORIENTED_EDGE('',*,*,#7631,.T.);
#9366=ORIENTED_EDGE('',*,*,#7595,.T.);
#9367=ORIENTED_EDGE('',*,*,#7592,.T.);
#9368=ORIENTED_EDGE('',*,*,#7589,.T.);
#9369=ORIENTED_EDGE('',*,*,#7586,.T.);
#9370=ORIENTED_EDGE('',*,*,#7583,.T.);
#9371=ORIENTED_EDGE('',*,*,#7630,.F.);
#9372=ORIENTED_EDGE('',*,*,#7632,.T.);
#9373=ORIENTED_EDGE('',*,*,#7633,.F.);
#9374=ORIENTED_EDGE('',*,*,#7632,.F.);
#9375=ORIENTED_EDGE('',*,*,#7631,.F.);
#9376=ORIENTED_EDGE('',*,*,#7634,.T.);
#9377=ORIENTED_EDGE('',*,*,#7635,.F.);
#9378=ORIENTED_EDGE('',*,*,#7634,.F.);
#9379=ORIENTED_EDGE('',*,*,#7614,.T.);
#9380=ORIENTED_EDGE('',*,*,#7626,.T.);
#9381=ORIENTED_EDGE('',*,*,#7636,.F.);
#9382=ORIENTED_EDGE('',*,*,#7637,.F.);
#9383=ORIENTED_EDGE('',*,*,#7635,.T.);
#9384=ORIENTED_EDGE('',*,*,#7633,.T.);
#9385=ORIENTED_EDGE('',*,*,#7597,.T.);
#9386=ORIENTED_EDGE('',*,*,#7594,.T.);
#9387=ORIENTED_EDGE('',*,*,#7591,.T.);
#9388=ORIENTED_EDGE('',*,*,#7588,.T.);
#9389=ORIENTED_EDGE('',*,*,#7585,.T.);
#9390=ORIENTED_EDGE('',*,*,#7637,.T.);
#9391=ORIENTED_EDGE('',*,*,#7638,.F.);
#9392=ORIENTED_EDGE('',*,*,#7628,.F.);
#9393=ORIENTED_EDGE('',*,*,#7613,.F.);
#9394=ORIENTED_EDGE('',*,*,#7622,.F.);
#9395=ORIENTED_EDGE('',*,*,#7639,.T.);
#9396=ORIENTED_EDGE('',*,*,#7620,.T.);
#9397=ORIENTED_EDGE('',*,*,#7615,.F.);
#9398=ORIENTED_EDGE('',*,*,#7629,.T.);
#9399=ORIENTED_EDGE('',*,*,#7638,.T.);
#9400=ORIENTED_EDGE('',*,*,#7636,.T.);
#9401=ORIENTED_EDGE('',*,*,#7625,.T.);
#9402=ORIENTED_EDGE('',*,*,#7627,.F.);
#9403=ORIENTED_EDGE('',*,*,#7618,.F.);
#9404=ORIENTED_EDGE('',*,*,#7639,.F.);
#9405=ORIENTED_EDGE('',*,*,#7621,.F.);
#9406=ORIENTED_EDGE('',*,*,#7598,.T.);
#9407=ORIENTED_EDGE('',*,*,#7601,.T.);
#9408=ORIENTED_EDGE('',*,*,#7604,.T.);
#9409=ORIENTED_EDGE('',*,*,#7607,.T.);
#9410=ORIENTED_EDGE('',*,*,#7640,.F.);
#9411=ORIENTED_EDGE('',*,*,#7641,.T.);
#9412=ORIENTED_EDGE('',*,*,#7642,.F.);
#9413=ORIENTED_EDGE('',*,*,#7641,.F.);
#9414=ORIENTED_EDGE('',*,*,#7643,.F.);
#9415=ORIENTED_EDGE('',*,*,#7644,.T.);
#9416=ORIENTED_EDGE('',*,*,#7645,.F.);
#9417=ORIENTED_EDGE('',*,*,#7644,.F.);
#9418=ORIENTED_EDGE('',*,*,#7646,.F.);
#9419=ORIENTED_EDGE('',*,*,#7647,.T.);
#9420=ORIENTED_EDGE('',*,*,#7648,.F.);
#9421=ORIENTED_EDGE('',*,*,#7647,.F.);
#9422=ORIENTED_EDGE('',*,*,#7649,.F.);
#9423=ORIENTED_EDGE('',*,*,#7650,.T.);
#9424=ORIENTED_EDGE('',*,*,#7651,.F.);
#9425=ORIENTED_EDGE('',*,*,#7650,.F.);
#9426=ORIENTED_EDGE('',*,*,#7652,.F.);
#9427=ORIENTED_EDGE('',*,*,#7653,.T.);
#9428=ORIENTED_EDGE('',*,*,#7654,.F.);
#9429=ORIENTED_EDGE('',*,*,#7653,.F.);
#9430=ORIENTED_EDGE('',*,*,#7652,.T.);
#9431=ORIENTED_EDGE('',*,*,#7655,.T.);
#9432=ORIENTED_EDGE('',*,*,#7655,.F.);
#9433=ORIENTED_EDGE('',*,*,#7656,.T.);
#9434=ORIENTED_EDGE('',*,*,#7657,.T.);
#9435=ORIENTED_EDGE('',*,*,#7656,.F.);
#9436=ORIENTED_EDGE('',*,*,#7658,.F.);
#9437=ORIENTED_EDGE('',*,*,#7659,.T.);
#9438=ORIENTED_EDGE('',*,*,#7660,.T.);
#9439=ORIENTED_EDGE('',*,*,#7659,.F.);
#9440=ORIENTED_EDGE('',*,*,#7658,.T.);
#9441=ORIENTED_EDGE('',*,*,#7654,.T.);
#9442=ORIENTED_EDGE('',*,*,#7651,.T.);
#9443=ORIENTED_EDGE('',*,*,#7648,.T.);
#9444=ORIENTED_EDGE('',*,*,#7645,.T.);
#9445=ORIENTED_EDGE('',*,*,#7642,.T.);
#9446=ORIENTED_EDGE('',*,*,#7660,.F.);
#9447=ORIENTED_EDGE('',*,*,#7657,.F.);
#9448=ORIENTED_EDGE('',*,*,#7649,.T.);
#9449=ORIENTED_EDGE('',*,*,#7646,.T.);
#9450=ORIENTED_EDGE('',*,*,#7643,.T.);
#9451=ORIENTED_EDGE('',*,*,#7640,.T.);
#9452=ORIENTED_EDGE('',*,*,#7661,.F.);
#9453=ORIENTED_EDGE('',*,*,#7662,.T.);
#9454=ORIENTED_EDGE('',*,*,#7663,.F.);
#9455=ORIENTED_EDGE('',*,*,#7662,.F.);
#9456=ORIENTED_EDGE('',*,*,#7664,.F.);
#9457=ORIENTED_EDGE('',*,*,#7665,.T.);
#9458=ORIENTED_EDGE('',*,*,#7666,.F.);
#9459=ORIENTED_EDGE('',*,*,#7665,.F.);
#9460=ORIENTED_EDGE('',*,*,#7667,.F.);
#9461=ORIENTED_EDGE('',*,*,#7668,.T.);
#9462=ORIENTED_EDGE('',*,*,#7669,.F.);
#9463=ORIENTED_EDGE('',*,*,#7668,.F.);
#9464=ORIENTED_EDGE('',*,*,#7670,.F.);
#9465=ORIENTED_EDGE('',*,*,#7671,.T.);
#9466=ORIENTED_EDGE('',*,*,#7672,.F.);
#9467=ORIENTED_EDGE('',*,*,#7671,.F.);
#9468=ORIENTED_EDGE('',*,*,#7673,.F.);
#9469=ORIENTED_EDGE('',*,*,#7674,.T.);
#9470=ORIENTED_EDGE('',*,*,#7675,.T.);
#9471=ORIENTED_EDGE('',*,*,#7674,.F.);
#9472=ORIENTED_EDGE('',*,*,#7675,.F.);
#9473=ORIENTED_EDGE('',*,*,#7676,.F.);
#9474=ORIENTED_EDGE('',*,*,#7677,.F.);
#9475=ORIENTED_EDGE('',*,*,#7678,.T.);
#9476=ORIENTED_EDGE('',*,*,#7676,.T.);
#9477=ORIENTED_EDGE('',*,*,#7678,.F.);
#9478=ORIENTED_EDGE('',*,*,#7679,.F.);
#9479=ORIENTED_EDGE('',*,*,#7680,.T.);
#9480=ORIENTED_EDGE('',*,*,#7681,.T.);
#9481=ORIENTED_EDGE('',*,*,#7680,.F.);
#9482=ORIENTED_EDGE('',*,*,#7679,.T.);
#9483=ORIENTED_EDGE('',*,*,#7677,.T.);
#9484=ORIENTED_EDGE('',*,*,#7672,.T.);
#9485=ORIENTED_EDGE('',*,*,#7669,.T.);
#9486=ORIENTED_EDGE('',*,*,#7666,.T.);
#9487=ORIENTED_EDGE('',*,*,#7663,.T.);
#9488=ORIENTED_EDGE('',*,*,#7681,.F.);
#9489=ORIENTED_EDGE('',*,*,#7673,.T.);
#9490=ORIENTED_EDGE('',*,*,#7670,.T.);
#9491=ORIENTED_EDGE('',*,*,#7667,.T.);
#9492=ORIENTED_EDGE('',*,*,#7664,.T.);
#9493=ORIENTED_EDGE('',*,*,#7661,.T.);
#9494=ORIENTED_EDGE('',*,*,#7682,.F.);
#9495=ORIENTED_EDGE('',*,*,#7683,.T.);
#9496=ORIENTED_EDGE('',*,*,#7684,.T.);
#9497=ORIENTED_EDGE('',*,*,#7683,.F.);
#9498=ORIENTED_EDGE('',*,*,#7682,.T.);
#9499=ORIENTED_EDGE('',*,*,#7684,.F.);
#9500=ORIENTED_EDGE('',*,*,#7685,.F.);
#9501=ORIENTED_EDGE('',*,*,#7686,.T.);
#9502=ORIENTED_EDGE('',*,*,#7687,.T.);
#9503=ORIENTED_EDGE('',*,*,#7686,.F.);
#9504=ORIENTED_EDGE('',*,*,#7685,.T.);
#9505=ORIENTED_EDGE('',*,*,#7687,.F.);
#9506=ORIENTED_EDGE('',*,*,#7688,.F.);
#9507=ORIENTED_EDGE('',*,*,#7689,.T.);
#9508=ORIENTED_EDGE('',*,*,#7690,.F.);
#9509=ORIENTED_EDGE('',*,*,#7689,.F.);
#9510=ORIENTED_EDGE('',*,*,#7688,.T.);
#9511=ORIENTED_EDGE('',*,*,#7691,.F.);
#9512=ORIENTED_EDGE('',*,*,#7692,.T.);
#9513=ORIENTED_EDGE('',*,*,#7693,.T.);
#9514=ORIENTED_EDGE('',*,*,#7692,.F.);
#9515=ORIENTED_EDGE('',*,*,#7693,.F.);
#9516=ORIENTED_EDGE('',*,*,#7694,.F.);
#9517=ORIENTED_EDGE('',*,*,#7695,.T.);
#9518=ORIENTED_EDGE('',*,*,#7696,.T.);
#9519=ORIENTED_EDGE('',*,*,#7695,.F.);
#9520=ORIENTED_EDGE('',*,*,#7694,.T.);
#9521=ORIENTED_EDGE('',*,*,#7690,.T.);
#9522=ORIENTED_EDGE('',*,*,#7696,.F.);
#9523=ORIENTED_EDGE('',*,*,#7691,.T.);
#9524=ORIENTED_EDGE('',*,*,#7697,.F.);
#9525=ORIENTED_EDGE('',*,*,#7698,.T.);
#9526=ORIENTED_EDGE('',*,*,#7699,.T.);
#9527=ORIENTED_EDGE('',*,*,#7698,.F.);
#9528=ORIENTED_EDGE('',*,*,#7700,.F.);
#9529=ORIENTED_EDGE('',*,*,#7701,.T.);
#9530=ORIENTED_EDGE('',*,*,#7702,.T.);
#9531=ORIENTED_EDGE('',*,*,#7701,.F.);
#9532=ORIENTED_EDGE('',*,*,#7700,.T.);
#9533=ORIENTED_EDGE('',*,*,#7697,.T.);
#9534=ORIENTED_EDGE('',*,*,#7702,.F.);
#9535=ORIENTED_EDGE('',*,*,#7699,.F.);
#9536=ORIENTED_EDGE('',*,*,#7703,.F.);
#9537=ORIENTED_EDGE('',*,*,#7704,.T.);
#9538=ORIENTED_EDGE('',*,*,#7705,.T.);
#9539=ORIENTED_EDGE('',*,*,#7704,.F.);
#9540=ORIENTED_EDGE('',*,*,#7706,.F.);
#9541=ORIENTED_EDGE('',*,*,#7707,.T.);
#9542=ORIENTED_EDGE('',*,*,#7708,.T.);
#9543=ORIENTED_EDGE('',*,*,#7707,.F.);
#9544=ORIENTED_EDGE('',*,*,#7706,.T.);
#9545=ORIENTED_EDGE('',*,*,#7703,.T.);
#9546=ORIENTED_EDGE('',*,*,#7708,.F.);
#9547=ORIENTED_EDGE('',*,*,#7705,.F.);
#9548=ORIENTED_EDGE('',*,*,#7709,.F.);
#9549=ORIENTED_EDGE('',*,*,#7710,.T.);
#9550=ORIENTED_EDGE('',*,*,#7711,.T.);
#9551=ORIENTED_EDGE('',*,*,#7710,.F.);
#9552=ORIENTED_EDGE('',*,*,#7712,.F.);
#9553=ORIENTED_EDGE('',*,*,#7713,.T.);
#9554=ORIENTED_EDGE('',*,*,#7714,.T.);
#9555=ORIENTED_EDGE('',*,*,#7713,.F.);
#9556=ORIENTED_EDGE('',*,*,#7712,.T.);
#9557=ORIENTED_EDGE('',*,*,#7709,.T.);
#9558=ORIENTED_EDGE('',*,*,#7714,.F.);
#9559=ORIENTED_EDGE('',*,*,#7711,.F.);
#9560=ORIENTED_EDGE('',*,*,#7715,.F.);
#9561=ORIENTED_EDGE('',*,*,#7716,.T.);
#9562=ORIENTED_EDGE('',*,*,#7717,.T.);
#9563=ORIENTED_EDGE('',*,*,#7716,.F.);
#9564=ORIENTED_EDGE('',*,*,#7718,.F.);
#9565=ORIENTED_EDGE('',*,*,#7719,.T.);
#9566=ORIENTED_EDGE('',*,*,#7720,.T.);
#9567=ORIENTED_EDGE('',*,*,#7719,.F.);
#9568=ORIENTED_EDGE('',*,*,#7718,.T.);
#9569=ORIENTED_EDGE('',*,*,#7715,.T.);
#9570=ORIENTED_EDGE('',*,*,#7720,.F.);
#9571=ORIENTED_EDGE('',*,*,#7717,.F.);
#9572=ORIENTED_EDGE('',*,*,#7721,.F.);
#9573=ORIENTED_EDGE('',*,*,#7722,.T.);
#9574=ORIENTED_EDGE('',*,*,#7723,.T.);
#9575=ORIENTED_EDGE('',*,*,#7722,.F.);
#9576=ORIENTED_EDGE('',*,*,#7724,.F.);
#9577=ORIENTED_EDGE('',*,*,#7725,.T.);
#9578=ORIENTED_EDGE('',*,*,#7726,.T.);
#9579=ORIENTED_EDGE('',*,*,#7725,.F.);
#9580=ORIENTED_EDGE('',*,*,#7724,.T.);
#9581=ORIENTED_EDGE('',*,*,#7721,.T.);
#9582=ORIENTED_EDGE('',*,*,#7726,.F.);
#9583=ORIENTED_EDGE('',*,*,#7723,.F.);
#9584=ORIENTED_EDGE('',*,*,#7727,.T.);
#9585=ORIENTED_EDGE('',*,*,#7728,.T.);
#9586=ORIENTED_EDGE('',*,*,#7729,.T.);
#9587=ORIENTED_EDGE('',*,*,#7730,.F.);
#9588=ORIENTED_EDGE('',*,*,#7731,.T.);
#9589=ORIENTED_EDGE('',*,*,#7732,.T.);
#9590=ORIENTED_EDGE('',*,*,#7733,.T.);
#9591=ORIENTED_EDGE('',*,*,#7728,.F.);
#9592=ORIENTED_EDGE('',*,*,#7734,.T.);
#9593=ORIENTED_EDGE('',*,*,#7735,.T.);
#9594=ORIENTED_EDGE('',*,*,#7736,.T.);
#9595=ORIENTED_EDGE('',*,*,#7732,.F.);
#9596=ORIENTED_EDGE('',*,*,#7737,.T.);
#9597=ORIENTED_EDGE('',*,*,#7738,.T.);
#9598=ORIENTED_EDGE('',*,*,#7739,.T.);
#9599=ORIENTED_EDGE('',*,*,#7735,.F.);
#9600=ORIENTED_EDGE('',*,*,#7740,.T.);
#9601=ORIENTED_EDGE('',*,*,#7741,.T.);
#9602=ORIENTED_EDGE('',*,*,#7742,.T.);
#9603=ORIENTED_EDGE('',*,*,#7738,.F.);
#9604=ORIENTED_EDGE('',*,*,#7743,.T.);
#9605=ORIENTED_EDGE('',*,*,#7730,.T.);
#9606=ORIENTED_EDGE('',*,*,#7744,.T.);
#9607=ORIENTED_EDGE('',*,*,#7741,.F.);
#9608=ORIENTED_EDGE('',*,*,#7743,.F.);
#9609=ORIENTED_EDGE('',*,*,#7740,.F.);
#9610=ORIENTED_EDGE('',*,*,#7737,.F.);
#9611=ORIENTED_EDGE('',*,*,#7734,.F.);
#9612=ORIENTED_EDGE('',*,*,#7731,.F.);
#9613=ORIENTED_EDGE('',*,*,#7727,.F.);
#9614=ORIENTED_EDGE('',*,*,#7744,.F.);
#9615=ORIENTED_EDGE('',*,*,#7729,.F.);
#9616=ORIENTED_EDGE('',*,*,#7733,.F.);
#9617=ORIENTED_EDGE('',*,*,#7736,.F.);
#9618=ORIENTED_EDGE('',*,*,#7739,.F.);
#9619=ORIENTED_EDGE('',*,*,#7742,.F.);
#9620=ORIENTED_EDGE('',*,*,#7745,.F.);
#9621=ORIENTED_EDGE('',*,*,#7746,.F.);
#9622=ORIENTED_EDGE('',*,*,#7747,.F.);
#9623=ORIENTED_EDGE('',*,*,#7748,.T.);
#9624=ORIENTED_EDGE('',*,*,#7746,.T.);
#9625=ORIENTED_EDGE('',*,*,#7748,.F.);
#9626=ORIENTED_EDGE('',*,*,#7749,.F.);
#9627=ORIENTED_EDGE('',*,*,#7750,.T.);
#9628=ORIENTED_EDGE('',*,*,#7747,.T.);
#9629=ORIENTED_EDGE('',*,*,#7750,.F.);
#9630=ORIENTED_EDGE('',*,*,#7751,.F.);
#9631=ORIENTED_EDGE('',*,*,#7752,.T.);
#9632=ORIENTED_EDGE('',*,*,#7749,.T.);
#9633=ORIENTED_EDGE('',*,*,#7752,.F.);
#9634=ORIENTED_EDGE('',*,*,#7751,.T.);
#9635=ORIENTED_EDGE('',*,*,#7753,.F.);
#9636=ORIENTED_EDGE('',*,*,#7754,.F.);
#9637=ORIENTED_EDGE('',*,*,#7755,.T.);
#9638=ORIENTED_EDGE('',*,*,#7753,.T.);
#9639=ORIENTED_EDGE('',*,*,#7755,.F.);
#9640=ORIENTED_EDGE('',*,*,#7745,.T.);
#9641=ORIENTED_EDGE('',*,*,#7756,.T.);
#9642=ORIENTED_EDGE('',*,*,#7754,.T.);
#9643=ORIENTED_EDGE('',*,*,#7756,.F.);
#9644=ORIENTED_EDGE('',*,*,#7757,.F.);
#9645=ORIENTED_EDGE('',*,*,#7758,.T.);
#9646=ORIENTED_EDGE('',*,*,#7759,.F.);
#9647=ORIENTED_EDGE('',*,*,#7758,.F.);
#9648=ORIENTED_EDGE('',*,*,#7760,.F.);
#9649=ORIENTED_EDGE('',*,*,#7761,.T.);
#9650=ORIENTED_EDGE('',*,*,#7762,.F.);
#9651=ORIENTED_EDGE('',*,*,#7761,.F.);
#9652=ORIENTED_EDGE('',*,*,#7763,.F.);
#9653=ORIENTED_EDGE('',*,*,#7764,.T.);
#9654=ORIENTED_EDGE('',*,*,#7765,.F.);
#9655=ORIENTED_EDGE('',*,*,#7764,.F.);
#9656=ORIENTED_EDGE('',*,*,#7766,.F.);
#9657=ORIENTED_EDGE('',*,*,#7767,.T.);
#9658=ORIENTED_EDGE('',*,*,#7768,.F.);
#9659=ORIENTED_EDGE('',*,*,#7767,.F.);
#9660=ORIENTED_EDGE('',*,*,#7769,.F.);
#9661=ORIENTED_EDGE('',*,*,#7770,.T.);
#9662=ORIENTED_EDGE('',*,*,#7771,.F.);
#9663=ORIENTED_EDGE('',*,*,#7770,.F.);
#9664=ORIENTED_EDGE('',*,*,#7772,.F.);
#9665=ORIENTED_EDGE('',*,*,#7773,.T.);
#9666=ORIENTED_EDGE('',*,*,#7774,.F.);
#9667=ORIENTED_EDGE('',*,*,#7773,.F.);
#9668=ORIENTED_EDGE('',*,*,#7775,.F.);
#9669=ORIENTED_EDGE('',*,*,#7776,.T.);
#9670=ORIENTED_EDGE('',*,*,#7777,.F.);
#9671=ORIENTED_EDGE('',*,*,#7776,.F.);
#9672=ORIENTED_EDGE('',*,*,#7778,.F.);
#9673=ORIENTED_EDGE('',*,*,#7779,.T.);
#9674=ORIENTED_EDGE('',*,*,#7780,.F.);
#9675=ORIENTED_EDGE('',*,*,#7779,.F.);
#9676=ORIENTED_EDGE('',*,*,#7781,.T.);
#9677=ORIENTED_EDGE('',*,*,#7782,.T.);
#9678=ORIENTED_EDGE('',*,*,#7783,.F.);
#9679=ORIENTED_EDGE('',*,*,#7784,.F.);
#9680=ORIENTED_EDGE('',*,*,#7785,.T.);
#9681=ORIENTED_EDGE('',*,*,#7784,.T.);
#9682=ORIENTED_EDGE('',*,*,#7786,.F.);
#9683=ORIENTED_EDGE('',*,*,#7787,.F.);
#9684=ORIENTED_EDGE('',*,*,#7788,.T.);
#9685=ORIENTED_EDGE('',*,*,#7787,.T.);
#9686=ORIENTED_EDGE('',*,*,#7789,.F.);
#9687=ORIENTED_EDGE('',*,*,#7790,.F.);
#9688=ORIENTED_EDGE('',*,*,#7791,.T.);
#9689=ORIENTED_EDGE('',*,*,#7790,.T.);
#9690=ORIENTED_EDGE('',*,*,#7792,.F.);
#9691=ORIENTED_EDGE('',*,*,#7782,.F.);
#9692=ORIENTED_EDGE('',*,*,#7792,.T.);
#9693=ORIENTED_EDGE('',*,*,#7789,.T.);
#9694=ORIENTED_EDGE('',*,*,#7786,.T.);
#9695=ORIENTED_EDGE('',*,*,#7783,.T.);
#9696=ORIENTED_EDGE('',*,*,#7780,.T.);
#9697=ORIENTED_EDGE('',*,*,#7777,.T.);
#9698=ORIENTED_EDGE('',*,*,#7774,.T.);
#9699=ORIENTED_EDGE('',*,*,#7771,.T.);
#9700=ORIENTED_EDGE('',*,*,#7768,.T.);
#9701=ORIENTED_EDGE('',*,*,#7765,.T.);
#9702=ORIENTED_EDGE('',*,*,#7762,.T.);
#9703=ORIENTED_EDGE('',*,*,#7759,.T.);
#9704=ORIENTED_EDGE('',*,*,#7791,.F.);
#9705=ORIENTED_EDGE('',*,*,#7781,.F.);
#9706=ORIENTED_EDGE('',*,*,#7785,.F.);
#9707=ORIENTED_EDGE('',*,*,#7788,.F.);
#9708=ORIENTED_EDGE('',*,*,#7778,.T.);
#9709=ORIENTED_EDGE('',*,*,#7775,.T.);
#9710=ORIENTED_EDGE('',*,*,#7772,.T.);
#9711=ORIENTED_EDGE('',*,*,#7769,.T.);
#9712=ORIENTED_EDGE('',*,*,#7766,.T.);
#9713=ORIENTED_EDGE('',*,*,#7763,.T.);
#9714=ORIENTED_EDGE('',*,*,#7760,.T.);
#9715=ORIENTED_EDGE('',*,*,#7757,.T.);
#9716=ORIENTED_EDGE('',*,*,#7793,.F.);
#9717=ORIENTED_EDGE('',*,*,#7794,.T.);
#9718=ORIENTED_EDGE('',*,*,#7795,.F.);
#9719=ORIENTED_EDGE('',*,*,#7794,.F.);
#9720=ORIENTED_EDGE('',*,*,#7796,.F.);
#9721=ORIENTED_EDGE('',*,*,#7797,.T.);
#9722=ORIENTED_EDGE('',*,*,#7798,.F.);
#9723=ORIENTED_EDGE('',*,*,#7797,.F.);
#9724=ORIENTED_EDGE('',*,*,#7799,.F.);
#9725=ORIENTED_EDGE('',*,*,#7800,.T.);
#9726=ORIENTED_EDGE('',*,*,#7801,.F.);
#9727=ORIENTED_EDGE('',*,*,#7800,.F.);
#9728=ORIENTED_EDGE('',*,*,#7802,.F.);
#9729=ORIENTED_EDGE('',*,*,#7803,.T.);
#9730=ORIENTED_EDGE('',*,*,#7804,.F.);
#9731=ORIENTED_EDGE('',*,*,#7803,.F.);
#9732=ORIENTED_EDGE('',*,*,#7805,.F.);
#9733=ORIENTED_EDGE('',*,*,#7806,.F.);
#9734=ORIENTED_EDGE('',*,*,#7807,.F.);
#9735=ORIENTED_EDGE('',*,*,#7808,.F.);
#9736=ORIENTED_EDGE('',*,*,#7809,.F.);
#9737=ORIENTED_EDGE('',*,*,#7810,.F.);
#9738=ORIENTED_EDGE('',*,*,#7811,.F.);
#9739=ORIENTED_EDGE('',*,*,#7812,.F.);
#9740=ORIENTED_EDGE('',*,*,#7802,.T.);
#9741=ORIENTED_EDGE('',*,*,#7799,.T.);
#9742=ORIENTED_EDGE('',*,*,#7796,.T.);
#9743=ORIENTED_EDGE('',*,*,#7793,.T.);
#9744=ORIENTED_EDGE('',*,*,#7806,.T.);
#9745=ORIENTED_EDGE('',*,*,#7813,.T.);
#9746=ORIENTED_EDGE('',*,*,#7814,.F.);
#9747=ORIENTED_EDGE('',*,*,#7815,.F.);
#9748=ORIENTED_EDGE('',*,*,#7807,.T.);
#9749=ORIENTED_EDGE('',*,*,#7815,.T.);
#9750=ORIENTED_EDGE('',*,*,#7816,.F.);
#9751=ORIENTED_EDGE('',*,*,#7817,.F.);
#9752=ORIENTED_EDGE('',*,*,#7808,.T.);
#9753=ORIENTED_EDGE('',*,*,#7817,.T.);
#9754=ORIENTED_EDGE('',*,*,#7818,.F.);
#9755=ORIENTED_EDGE('',*,*,#7819,.F.);
#9756=ORIENTED_EDGE('',*,*,#7805,.T.);
#9757=ORIENTED_EDGE('',*,*,#7819,.T.);
#9758=ORIENTED_EDGE('',*,*,#7820,.F.);
#9759=ORIENTED_EDGE('',*,*,#7813,.F.);
#9760=ORIENTED_EDGE('',*,*,#7811,.T.);
#9761=ORIENTED_EDGE('',*,*,#7821,.F.);
#9762=ORIENTED_EDGE('',*,*,#7822,.T.);
#9763=ORIENTED_EDGE('',*,*,#7823,.T.);
#9764=ORIENTED_EDGE('',*,*,#7824,.T.);
#9765=ORIENTED_EDGE('',*,*,#7810,.T.);
#9766=ORIENTED_EDGE('',*,*,#7825,.F.);
#9767=ORIENTED_EDGE('',*,*,#7826,.T.);
#9768=ORIENTED_EDGE('',*,*,#7821,.T.);
#9769=ORIENTED_EDGE('',*,*,#7827,.T.);
#9770=ORIENTED_EDGE('',*,*,#7828,.T.);
#9771=ORIENTED_EDGE('',*,*,#7824,.F.);
#9772=ORIENTED_EDGE('',*,*,#7829,.T.);
#9773=ORIENTED_EDGE('',*,*,#7830,.F.);
#9774=ORIENTED_EDGE('',*,*,#7829,.F.);
#9775=ORIENTED_EDGE('',*,*,#7828,.F.);
#9776=ORIENTED_EDGE('',*,*,#7831,.T.);
#9777=ORIENTED_EDGE('',*,*,#7832,.F.);
#9778=ORIENTED_EDGE('',*,*,#7831,.F.);
#9779=ORIENTED_EDGE('',*,*,#7827,.F.);
#9780=ORIENTED_EDGE('',*,*,#7833,.T.);
#9781=ORIENTED_EDGE('',*,*,#7834,.F.);
#9782=ORIENTED_EDGE('',*,*,#7833,.F.);
#9783=ORIENTED_EDGE('',*,*,#7809,.T.);
#9784=ORIENTED_EDGE('',*,*,#7835,.F.);
#9785=ORIENTED_EDGE('',*,*,#7836,.T.);
#9786=ORIENTED_EDGE('',*,*,#7825,.T.);
#9787=ORIENTED_EDGE('',*,*,#7830,.T.);
#9788=ORIENTED_EDGE('',*,*,#7812,.T.);
#9789=ORIENTED_EDGE('',*,*,#7823,.F.);
#9790=ORIENTED_EDGE('',*,*,#7837,.T.);
#9791=ORIENTED_EDGE('',*,*,#7835,.T.);
#9792=ORIENTED_EDGE('',*,*,#7832,.T.);
#9793=ORIENTED_EDGE('',*,*,#7834,.T.);
#9794=ORIENTED_EDGE('',*,*,#7820,.T.);
#9795=ORIENTED_EDGE('',*,*,#7818,.T.);
#9796=ORIENTED_EDGE('',*,*,#7816,.T.);
#9797=ORIENTED_EDGE('',*,*,#7814,.T.);
#9798=ORIENTED_EDGE('',*,*,#7795,.T.);
#9799=ORIENTED_EDGE('',*,*,#7798,.T.);
#9800=ORIENTED_EDGE('',*,*,#7801,.T.);
#9801=ORIENTED_EDGE('',*,*,#7804,.T.);
#9802=ORIENTED_EDGE('',*,*,#7826,.F.);
#9803=ORIENTED_EDGE('',*,*,#7836,.F.);
#9804=ORIENTED_EDGE('',*,*,#7837,.F.);
#9805=ORIENTED_EDGE('',*,*,#7822,.F.);
#9806=ORIENTED_EDGE('',*,*,#7838,.F.);
#9807=ORIENTED_EDGE('',*,*,#7839,.T.);
#9808=ORIENTED_EDGE('',*,*,#7840,.F.);
#9809=ORIENTED_EDGE('',*,*,#7839,.F.);
#9810=ORIENTED_EDGE('',*,*,#7841,.F.);
#9811=ORIENTED_EDGE('',*,*,#7842,.T.);
#9812=ORIENTED_EDGE('',*,*,#7843,.F.);
#9813=ORIENTED_EDGE('',*,*,#7842,.F.);
#9814=ORIENTED_EDGE('',*,*,#7844,.F.);
#9815=ORIENTED_EDGE('',*,*,#7845,.T.);
#9816=ORIENTED_EDGE('',*,*,#7846,.F.);
#9817=ORIENTED_EDGE('',*,*,#7845,.F.);
#9818=ORIENTED_EDGE('',*,*,#7847,.F.);
#9819=ORIENTED_EDGE('',*,*,#7848,.T.);
#9820=ORIENTED_EDGE('',*,*,#7849,.F.);
#9821=ORIENTED_EDGE('',*,*,#7848,.F.);
#9822=ORIENTED_EDGE('',*,*,#7850,.F.);
#9823=ORIENTED_EDGE('',*,*,#7851,.F.);
#9824=ORIENTED_EDGE('',*,*,#7852,.F.);
#9825=ORIENTED_EDGE('',*,*,#7853,.F.);
#9826=ORIENTED_EDGE('',*,*,#7841,.T.);
#9827=ORIENTED_EDGE('',*,*,#7844,.T.);
#9828=ORIENTED_EDGE('',*,*,#7854,.T.);
#9829=ORIENTED_EDGE('',*,*,#7855,.T.);
#9830=ORIENTED_EDGE('',*,*,#7856,.F.);
#9831=ORIENTED_EDGE('',*,*,#7857,.F.);
#9832=ORIENTED_EDGE('',*,*,#7852,.T.);
#9833=ORIENTED_EDGE('',*,*,#7858,.T.);
#9834=ORIENTED_EDGE('',*,*,#7859,.F.);
#9835=ORIENTED_EDGE('',*,*,#7860,.F.);
#9836=ORIENTED_EDGE('',*,*,#7861,.F.);
#9837=ORIENTED_EDGE('',*,*,#7862,.F.);
#9838=ORIENTED_EDGE('',*,*,#7854,.F.);
#9839=ORIENTED_EDGE('',*,*,#7863,.F.);
#9840=ORIENTED_EDGE('',*,*,#7838,.T.);
#9841=ORIENTED_EDGE('',*,*,#7847,.T.);
#9842=ORIENTED_EDGE('',*,*,#7861,.T.);
#9843=ORIENTED_EDGE('',*,*,#7864,.F.);
#9844=ORIENTED_EDGE('',*,*,#7865,.T.);
#9845=ORIENTED_EDGE('',*,*,#7866,.T.);
#9846=ORIENTED_EDGE('',*,*,#7867,.T.);
#9847=ORIENTED_EDGE('',*,*,#7868,.T.);
#9848=ORIENTED_EDGE('',*,*,#7869,.F.);
#9849=ORIENTED_EDGE('',*,*,#7870,.T.);
#9850=ORIENTED_EDGE('',*,*,#7864,.T.);
#9851=ORIENTED_EDGE('',*,*,#7863,.T.);
#9852=ORIENTED_EDGE('',*,*,#7857,.T.);
#9853=ORIENTED_EDGE('',*,*,#7871,.F.);
#9854=ORIENTED_EDGE('',*,*,#7858,.F.);
#9855=ORIENTED_EDGE('',*,*,#7851,.T.);
#9856=ORIENTED_EDGE('',*,*,#7872,.F.);
#9857=ORIENTED_EDGE('',*,*,#7873,.T.);
#9858=ORIENTED_EDGE('',*,*,#7868,.F.);
#9859=ORIENTED_EDGE('',*,*,#7873,.F.);
#9860=ORIENTED_EDGE('',*,*,#7874,.F.);
#9861=ORIENTED_EDGE('',*,*,#7875,.T.);
#9862=ORIENTED_EDGE('',*,*,#7867,.F.);
#9863=ORIENTED_EDGE('',*,*,#7875,.F.);
#9864=ORIENTED_EDGE('',*,*,#7866,.F.);
#9865=ORIENTED_EDGE('',*,*,#7876,.T.);
#9866=ORIENTED_EDGE('',*,*,#7877,.T.);
#9867=ORIENTED_EDGE('',*,*,#7853,.T.);
#9868=ORIENTED_EDGE('',*,*,#7860,.T.);
#9869=ORIENTED_EDGE('',*,*,#7878,.F.);
#9870=ORIENTED_EDGE('',*,*,#7855,.F.);
#9871=ORIENTED_EDGE('',*,*,#7862,.T.);
#9872=ORIENTED_EDGE('',*,*,#7850,.T.);
#9873=ORIENTED_EDGE('',*,*,#7877,.F.);
#9874=ORIENTED_EDGE('',*,*,#7879,.T.);
#9875=ORIENTED_EDGE('',*,*,#7869,.T.);
#9876=ORIENTED_EDGE('',*,*,#7872,.T.);
#9877=ORIENTED_EDGE('',*,*,#7874,.T.);
#9878=ORIENTED_EDGE('',*,*,#7871,.T.);
#9879=ORIENTED_EDGE('',*,*,#7856,.T.);
#9880=ORIENTED_EDGE('',*,*,#7878,.T.);
#9881=ORIENTED_EDGE('',*,*,#7859,.T.);
#9882=ORIENTED_EDGE('',*,*,#7840,.T.);
#9883=ORIENTED_EDGE('',*,*,#7843,.T.);
#9884=ORIENTED_EDGE('',*,*,#7846,.T.);
#9885=ORIENTED_EDGE('',*,*,#7849,.T.);
#9886=ORIENTED_EDGE('',*,*,#7879,.F.);
#9887=ORIENTED_EDGE('',*,*,#7876,.F.);
#9888=ORIENTED_EDGE('',*,*,#7865,.F.);
#9889=ORIENTED_EDGE('',*,*,#7870,.F.);
#9890=ORIENTED_EDGE('',*,*,#7880,.F.);
#9891=ORIENTED_EDGE('',*,*,#7881,.T.);
#9892=ORIENTED_EDGE('',*,*,#7882,.T.);
#9893=ORIENTED_EDGE('',*,*,#7881,.F.);
#9894=ORIENTED_EDGE('',*,*,#7880,.T.);
#9895=ORIENTED_EDGE('',*,*,#7882,.F.);
#9896=ORIENTED_EDGE('',*,*,#7883,.F.);
#9897=ORIENTED_EDGE('',*,*,#7884,.T.);
#9898=ORIENTED_EDGE('',*,*,#7885,.T.);
#9899=ORIENTED_EDGE('',*,*,#7884,.F.);
#9900=ORIENTED_EDGE('',*,*,#7883,.T.);
#9901=ORIENTED_EDGE('',*,*,#7885,.F.);
#9902=ORIENTED_EDGE('',*,*,#7886,.F.);
#9903=ORIENTED_EDGE('',*,*,#7887,.T.);
#9904=ORIENTED_EDGE('',*,*,#7888,.F.);
#9905=ORIENTED_EDGE('',*,*,#7887,.F.);
#9906=ORIENTED_EDGE('',*,*,#7886,.T.);
#9907=ORIENTED_EDGE('',*,*,#7889,.F.);
#9908=ORIENTED_EDGE('',*,*,#7890,.T.);
#9909=ORIENTED_EDGE('',*,*,#7891,.T.);
#9910=ORIENTED_EDGE('',*,*,#7890,.F.);
#9911=ORIENTED_EDGE('',*,*,#7891,.F.);
#9912=ORIENTED_EDGE('',*,*,#7892,.F.);
#9913=ORIENTED_EDGE('',*,*,#7893,.T.);
#9914=ORIENTED_EDGE('',*,*,#7894,.T.);
#9915=ORIENTED_EDGE('',*,*,#7893,.F.);
#9916=ORIENTED_EDGE('',*,*,#7892,.T.);
#9917=ORIENTED_EDGE('',*,*,#7888,.T.);
#9918=ORIENTED_EDGE('',*,*,#7894,.F.);
#9919=ORIENTED_EDGE('',*,*,#7889,.T.);
#9920=ORIENTED_EDGE('',*,*,#7895,.F.);
#9921=ORIENTED_EDGE('',*,*,#7896,.T.);
#9922=ORIENTED_EDGE('',*,*,#7897,.T.);
#9923=ORIENTED_EDGE('',*,*,#7896,.F.);
#9924=ORIENTED_EDGE('',*,*,#7898,.F.);
#9925=ORIENTED_EDGE('',*,*,#7899,.T.);
#9926=ORIENTED_EDGE('',*,*,#7900,.T.);
#9927=ORIENTED_EDGE('',*,*,#7899,.F.);
#9928=ORIENTED_EDGE('',*,*,#7898,.T.);
#9929=ORIENTED_EDGE('',*,*,#7895,.T.);
#9930=ORIENTED_EDGE('',*,*,#7900,.F.);
#9931=ORIENTED_EDGE('',*,*,#7897,.F.);
#9932=ORIENTED_EDGE('',*,*,#7901,.F.);
#9933=ORIENTED_EDGE('',*,*,#7902,.T.);
#9934=ORIENTED_EDGE('',*,*,#7903,.T.);
#9935=ORIENTED_EDGE('',*,*,#7902,.F.);
#9936=ORIENTED_EDGE('',*,*,#7904,.F.);
#9937=ORIENTED_EDGE('',*,*,#7905,.T.);
#9938=ORIENTED_EDGE('',*,*,#7906,.T.);
#9939=ORIENTED_EDGE('',*,*,#7905,.F.);
#9940=ORIENTED_EDGE('',*,*,#7904,.T.);
#9941=ORIENTED_EDGE('',*,*,#7901,.T.);
#9942=ORIENTED_EDGE('',*,*,#7906,.F.);
#9943=ORIENTED_EDGE('',*,*,#7903,.F.);
#9944=ORIENTED_EDGE('',*,*,#7907,.F.);
#9945=ORIENTED_EDGE('',*,*,#7908,.T.);
#9946=ORIENTED_EDGE('',*,*,#7909,.T.);
#9947=ORIENTED_EDGE('',*,*,#7908,.F.);
#9948=ORIENTED_EDGE('',*,*,#7910,.F.);
#9949=ORIENTED_EDGE('',*,*,#7911,.T.);
#9950=ORIENTED_EDGE('',*,*,#7912,.T.);
#9951=ORIENTED_EDGE('',*,*,#7911,.F.);
#9952=ORIENTED_EDGE('',*,*,#7910,.T.);
#9953=ORIENTED_EDGE('',*,*,#7907,.T.);
#9954=ORIENTED_EDGE('',*,*,#7912,.F.);
#9955=ORIENTED_EDGE('',*,*,#7909,.F.);
#9956=ORIENTED_EDGE('',*,*,#7913,.F.);
#9957=ORIENTED_EDGE('',*,*,#7914,.T.);
#9958=ORIENTED_EDGE('',*,*,#7915,.T.);
#9959=ORIENTED_EDGE('',*,*,#7914,.F.);
#9960=ORIENTED_EDGE('',*,*,#7916,.F.);
#9961=ORIENTED_EDGE('',*,*,#7917,.T.);
#9962=ORIENTED_EDGE('',*,*,#7918,.T.);
#9963=ORIENTED_EDGE('',*,*,#7917,.F.);
#9964=ORIENTED_EDGE('',*,*,#7916,.T.);
#9965=ORIENTED_EDGE('',*,*,#7913,.T.);
#9966=ORIENTED_EDGE('',*,*,#7918,.F.);
#9967=ORIENTED_EDGE('',*,*,#7915,.F.);
#9968=ORIENTED_EDGE('',*,*,#7919,.F.);
#9969=ORIENTED_EDGE('',*,*,#7920,.T.);
#9970=ORIENTED_EDGE('',*,*,#7921,.T.);
#9971=ORIENTED_EDGE('',*,*,#7920,.F.);
#9972=ORIENTED_EDGE('',*,*,#7922,.F.);
#9973=ORIENTED_EDGE('',*,*,#7923,.T.);
#9974=ORIENTED_EDGE('',*,*,#7924,.T.);
#9975=ORIENTED_EDGE('',*,*,#7923,.F.);
#9976=ORIENTED_EDGE('',*,*,#7922,.T.);
#9977=ORIENTED_EDGE('',*,*,#7919,.T.);
#9978=ORIENTED_EDGE('',*,*,#7924,.F.);
#9979=ORIENTED_EDGE('',*,*,#7921,.F.);
#9980=ORIENTED_EDGE('',*,*,#7925,.F.);
#9981=ORIENTED_EDGE('',*,*,#7926,.T.);
#9982=ORIENTED_EDGE('',*,*,#7927,.T.);
#9983=ORIENTED_EDGE('',*,*,#7926,.F.);
#9984=ORIENTED_EDGE('',*,*,#7928,.F.);
#9985=ORIENTED_EDGE('',*,*,#7929,.T.);
#9986=ORIENTED_EDGE('',*,*,#7930,.T.);
#9987=ORIENTED_EDGE('',*,*,#7929,.F.);
#9988=ORIENTED_EDGE('',*,*,#7928,.T.);
#9989=ORIENTED_EDGE('',*,*,#7925,.T.);
#9990=ORIENTED_EDGE('',*,*,#7930,.F.);
#9991=ORIENTED_EDGE('',*,*,#7927,.F.);
#9992=ORIENTED_EDGE('',*,*,#7931,.F.);
#9993=ORIENTED_EDGE('',*,*,#7932,.F.);
#9994=ORIENTED_EDGE('',*,*,#7933,.T.);
#9995=ORIENTED_EDGE('',*,*,#7931,.T.);
#9996=ORIENTED_EDGE('',*,*,#7933,.F.);
#9997=ORIENTED_EDGE('',*,*,#7934,.F.);
#9998=ORIENTED_EDGE('',*,*,#7935,.T.);
#9999=ORIENTED_EDGE('',*,*,#7932,.T.);
#10000=ORIENTED_EDGE('',*,*,#7935,.F.);
#10001=ORIENTED_EDGE('',*,*,#7936,.F.);
#10002=ORIENTED_EDGE('',*,*,#7937,.T.);
#10003=ORIENTED_EDGE('',*,*,#7934,.T.);
#10004=ORIENTED_EDGE('',*,*,#7937,.F.);
#10005=ORIENTED_EDGE('',*,*,#7936,.T.);
#10006=ORIENTED_EDGE('',*,*,#7938,.F.);
#10007=ORIENTED_EDGE('',*,*,#7939,.F.);
#10008=ORIENTED_EDGE('',*,*,#7940,.T.);
#10009=ORIENTED_EDGE('',*,*,#7938,.T.);
#10010=ORIENTED_EDGE('',*,*,#7940,.F.);
#10011=ORIENTED_EDGE('',*,*,#7941,.F.);
#10012=ORIENTED_EDGE('',*,*,#7942,.T.);
#10013=ORIENTED_EDGE('',*,*,#7939,.T.);
#10014=ORIENTED_EDGE('',*,*,#7942,.F.);
#10015=ORIENTED_EDGE('',*,*,#7943,.F.);
#10016=ORIENTED_EDGE('',*,*,#7944,.T.);
#10017=ORIENTED_EDGE('',*,*,#7941,.T.);
#10018=ORIENTED_EDGE('',*,*,#7944,.F.);
#10019=ORIENTED_EDGE('',*,*,#7943,.T.);
#10020=ORIENTED_EDGE('',*,*,#7945,.T.);
#10021=ORIENTED_EDGE('',*,*,#7946,.T.);
#10022=ORIENTED_EDGE('',*,*,#7947,.T.);
#10023=ORIENTED_EDGE('',*,*,#7948,.F.);
#10024=ORIENTED_EDGE('',*,*,#7949,.T.);
#10025=ORIENTED_EDGE('',*,*,#7950,.T.);
#10026=ORIENTED_EDGE('',*,*,#7951,.T.);
#10027=ORIENTED_EDGE('',*,*,#7946,.F.);
#10028=ORIENTED_EDGE('',*,*,#7952,.T.);
#10029=ORIENTED_EDGE('',*,*,#7953,.T.);
#10030=ORIENTED_EDGE('',*,*,#7954,.T.);
#10031=ORIENTED_EDGE('',*,*,#7950,.F.);
#10032=ORIENTED_EDGE('',*,*,#7955,.T.);
#10033=ORIENTED_EDGE('',*,*,#7956,.T.);
#10034=ORIENTED_EDGE('',*,*,#7957,.T.);
#10035=ORIENTED_EDGE('',*,*,#7953,.F.);
#10036=ORIENTED_EDGE('',*,*,#7958,.T.);
#10037=ORIENTED_EDGE('',*,*,#7959,.T.);
#10038=ORIENTED_EDGE('',*,*,#7960,.T.);
#10039=ORIENTED_EDGE('',*,*,#7956,.F.);
#10040=ORIENTED_EDGE('',*,*,#7961,.T.);
#10041=ORIENTED_EDGE('',*,*,#7948,.T.);
#10042=ORIENTED_EDGE('',*,*,#7962,.T.);
#10043=ORIENTED_EDGE('',*,*,#7959,.F.);
#10044=ORIENTED_EDGE('',*,*,#7961,.F.);
#10045=ORIENTED_EDGE('',*,*,#7958,.F.);
#10046=ORIENTED_EDGE('',*,*,#7955,.F.);
#10047=ORIENTED_EDGE('',*,*,#7952,.F.);
#10048=ORIENTED_EDGE('',*,*,#7949,.F.);
#10049=ORIENTED_EDGE('',*,*,#7945,.F.);
#10050=ORIENTED_EDGE('',*,*,#7962,.F.);
#10051=ORIENTED_EDGE('',*,*,#7947,.F.);
#10052=ORIENTED_EDGE('',*,*,#7951,.F.);
#10053=ORIENTED_EDGE('',*,*,#7954,.F.);
#10054=ORIENTED_EDGE('',*,*,#7957,.F.);
#10055=ORIENTED_EDGE('',*,*,#7960,.F.);
#10056=ORIENTED_EDGE('',*,*,#7963,.F.);
#10057=ORIENTED_EDGE('',*,*,#7964,.T.);
#10058=ORIENTED_EDGE('',*,*,#7965,.F.);
#10059=ORIENTED_EDGE('',*,*,#7964,.F.);
#10060=ORIENTED_EDGE('',*,*,#7966,.F.);
#10061=ORIENTED_EDGE('',*,*,#7967,.T.);
#10062=ORIENTED_EDGE('',*,*,#7968,.F.);
#10063=ORIENTED_EDGE('',*,*,#7967,.F.);
#10064=ORIENTED_EDGE('',*,*,#7969,.F.);
#10065=ORIENTED_EDGE('',*,*,#7970,.T.);
#10066=ORIENTED_EDGE('',*,*,#7971,.F.);
#10067=ORIENTED_EDGE('',*,*,#7970,.F.);
#10068=ORIENTED_EDGE('',*,*,#7972,.T.);
#10069=ORIENTED_EDGE('',*,*,#7973,.T.);
#10070=ORIENTED_EDGE('',*,*,#7974,.F.);
#10071=ORIENTED_EDGE('',*,*,#7975,.F.);
#10072=ORIENTED_EDGE('',*,*,#7976,.T.);
#10073=ORIENTED_EDGE('',*,*,#7975,.T.);
#10074=ORIENTED_EDGE('',*,*,#7977,.F.);
#10075=ORIENTED_EDGE('',*,*,#7978,.F.);
#10076=ORIENTED_EDGE('',*,*,#7965,.T.);
#10077=ORIENTED_EDGE('',*,*,#7968,.T.);
#10078=ORIENTED_EDGE('',*,*,#7971,.T.);
#10079=ORIENTED_EDGE('',*,*,#7979,.T.);
#10080=ORIENTED_EDGE('',*,*,#7978,.T.);
#10081=ORIENTED_EDGE('',*,*,#7980,.F.);
#10082=ORIENTED_EDGE('',*,*,#7981,.F.);
#10083=ORIENTED_EDGE('',*,*,#7982,.T.);
#10084=ORIENTED_EDGE('',*,*,#7981,.T.);
#10085=ORIENTED_EDGE('',*,*,#7983,.F.);
#10086=ORIENTED_EDGE('',*,*,#7973,.F.);
#10087=ORIENTED_EDGE('',*,*,#7963,.T.);
#10088=ORIENTED_EDGE('',*,*,#7966,.T.);
#10089=ORIENTED_EDGE('',*,*,#7969,.T.);
#10090=ORIENTED_EDGE('',*,*,#7983,.T.);
#10091=ORIENTED_EDGE('',*,*,#7980,.T.);
#10092=ORIENTED_EDGE('',*,*,#7977,.T.);
#10093=ORIENTED_EDGE('',*,*,#7974,.T.);
#10094=ORIENTED_EDGE('',*,*,#7982,.F.);
#10095=ORIENTED_EDGE('',*,*,#7972,.F.);
#10096=ORIENTED_EDGE('',*,*,#7976,.F.);
#10097=ORIENTED_EDGE('',*,*,#7979,.F.);
#10098=ORIENTED_EDGE('',*,*,#7984,.F.);
#10099=ORIENTED_EDGE('',*,*,#7985,.T.);
#10100=ORIENTED_EDGE('',*,*,#7986,.F.);
#10101=ORIENTED_EDGE('',*,*,#7985,.F.);
#10102=ORIENTED_EDGE('',*,*,#7984,.T.);
#10103=ORIENTED_EDGE('',*,*,#7987,.T.);
#10104=ORIENTED_EDGE('',*,*,#7988,.F.);
#10105=ORIENTED_EDGE('',*,*,#7989,.T.);
#10106=ORIENTED_EDGE('',*,*,#7990,.F.);
#10107=ORIENTED_EDGE('',*,*,#7989,.F.);
#10108=ORIENTED_EDGE('',*,*,#7988,.T.);
#10109=ORIENTED_EDGE('',*,*,#7991,.T.);
#10110=ORIENTED_EDGE('',*,*,#7992,.F.);
#10111=ORIENTED_EDGE('',*,*,#7993,.T.);
#10112=ORIENTED_EDGE('',*,*,#7994,.F.);
#10113=ORIENTED_EDGE('',*,*,#7993,.F.);
#10114=ORIENTED_EDGE('',*,*,#7995,.F.);
#10115=ORIENTED_EDGE('',*,*,#7996,.T.);
#10116=ORIENTED_EDGE('',*,*,#7991,.F.);
#10117=ORIENTED_EDGE('',*,*,#7996,.F.);
#10118=ORIENTED_EDGE('',*,*,#7997,.F.);
#10119=ORIENTED_EDGE('',*,*,#7998,.T.);
#10120=ORIENTED_EDGE('',*,*,#7987,.F.);
#10121=ORIENTED_EDGE('',*,*,#7998,.F.);
#10122=ORIENTED_EDGE('',*,*,#7999,.T.);
#10123=ORIENTED_EDGE('',*,*,#8000,.T.);
#10124=ORIENTED_EDGE('',*,*,#8001,.F.);
#10125=ORIENTED_EDGE('',*,*,#8002,.F.);
#10126=ORIENTED_EDGE('',*,*,#8003,.T.);
#10127=ORIENTED_EDGE('',*,*,#8002,.T.);
#10128=ORIENTED_EDGE('',*,*,#8004,.F.);
#10129=ORIENTED_EDGE('',*,*,#8005,.F.);
#10130=ORIENTED_EDGE('',*,*,#8006,.T.);
#10131=ORIENTED_EDGE('',*,*,#8005,.T.);
#10132=ORIENTED_EDGE('',*,*,#8007,.F.);
#10133=ORIENTED_EDGE('',*,*,#8008,.F.);
#10134=ORIENTED_EDGE('',*,*,#8009,.T.);
#10135=ORIENTED_EDGE('',*,*,#8008,.T.);
#10136=ORIENTED_EDGE('',*,*,#8010,.F.);
#10137=ORIENTED_EDGE('',*,*,#8000,.F.);
#10138=ORIENTED_EDGE('',*,*,#8010,.T.);
#10139=ORIENTED_EDGE('',*,*,#8007,.T.);
#10140=ORIENTED_EDGE('',*,*,#8004,.T.);
#10141=ORIENTED_EDGE('',*,*,#8001,.T.);
#10142=ORIENTED_EDGE('',*,*,#7986,.T.);
#10143=ORIENTED_EDGE('',*,*,#7990,.T.);
#10144=ORIENTED_EDGE('',*,*,#7994,.T.);
#10145=ORIENTED_EDGE('',*,*,#8009,.F.);
#10146=ORIENTED_EDGE('',*,*,#7999,.F.);
#10147=ORIENTED_EDGE('',*,*,#8003,.F.);
#10148=ORIENTED_EDGE('',*,*,#8006,.F.);
#10149=ORIENTED_EDGE('',*,*,#7992,.T.);
#10150=ORIENTED_EDGE('',*,*,#7995,.T.);
#10151=ORIENTED_EDGE('',*,*,#7997,.T.);
#10152=ORIENTED_EDGE('',*,*,#8011,.F.);
#10153=ORIENTED_EDGE('',*,*,#8012,.T.);
#10154=ORIENTED_EDGE('',*,*,#8013,.T.);
#10155=ORIENTED_EDGE('',*,*,#8012,.F.);
#10156=ORIENTED_EDGE('',*,*,#8013,.F.);
#10157=ORIENTED_EDGE('',*,*,#8014,.F.);
#10158=ORIENTED_EDGE('',*,*,#8015,.F.);
#10159=ORIENTED_EDGE('',*,*,#8016,.T.);
#10160=ORIENTED_EDGE('',*,*,#8017,.T.);
#10161=ORIENTED_EDGE('',*,*,#8016,.F.);
#10162=ORIENTED_EDGE('',*,*,#8017,.F.);
#10163=ORIENTED_EDGE('',*,*,#8018,.F.);
#10164=ORIENTED_EDGE('',*,*,#8019,.F.);
#10165=ORIENTED_EDGE('',*,*,#8020,.T.);
#10166=ORIENTED_EDGE('',*,*,#8021,.F.);
#10167=ORIENTED_EDGE('',*,*,#8020,.F.);
#10168=ORIENTED_EDGE('',*,*,#8018,.T.);
#10169=ORIENTED_EDGE('',*,*,#8022,.T.);
#10170=ORIENTED_EDGE('',*,*,#8023,.F.);
#10171=ORIENTED_EDGE('',*,*,#8022,.F.);
#10172=ORIENTED_EDGE('',*,*,#8014,.T.);
#10173=ORIENTED_EDGE('',*,*,#8024,.T.);
#10174=ORIENTED_EDGE('',*,*,#8025,.F.);
#10175=ORIENTED_EDGE('',*,*,#8024,.F.);
#10176=ORIENTED_EDGE('',*,*,#8026,.T.);
#10177=ORIENTED_EDGE('',*,*,#8027,.T.);
#10178=ORIENTED_EDGE('',*,*,#8028,.F.);
#10179=ORIENTED_EDGE('',*,*,#8029,.F.);
#10180=ORIENTED_EDGE('',*,*,#8030,.T.);
#10181=ORIENTED_EDGE('',*,*,#8029,.T.);
#10182=ORIENTED_EDGE('',*,*,#8031,.F.);
#10183=ORIENTED_EDGE('',*,*,#8032,.F.);
#10184=ORIENTED_EDGE('',*,*,#8033,.T.);
#10185=ORIENTED_EDGE('',*,*,#8032,.T.);
#10186=ORIENTED_EDGE('',*,*,#8034,.F.);
#10187=ORIENTED_EDGE('',*,*,#8035,.F.);
#10188=ORIENTED_EDGE('',*,*,#8036,.T.);
#10189=ORIENTED_EDGE('',*,*,#8035,.T.);
#10190=ORIENTED_EDGE('',*,*,#8037,.F.);
#10191=ORIENTED_EDGE('',*,*,#8027,.F.);
#10192=ORIENTED_EDGE('',*,*,#8037,.T.);
#10193=ORIENTED_EDGE('',*,*,#8034,.T.);
#10194=ORIENTED_EDGE('',*,*,#8031,.T.);
#10195=ORIENTED_EDGE('',*,*,#8028,.T.);
#10196=ORIENTED_EDGE('',*,*,#8021,.T.);
#10197=ORIENTED_EDGE('',*,*,#8023,.T.);
#10198=ORIENTED_EDGE('',*,*,#8025,.T.);
#10199=ORIENTED_EDGE('',*,*,#8036,.F.);
#10200=ORIENTED_EDGE('',*,*,#8026,.F.);
#10201=ORIENTED_EDGE('',*,*,#8030,.F.);
#10202=ORIENTED_EDGE('',*,*,#8033,.F.);
#10203=ORIENTED_EDGE('',*,*,#8011,.T.);
#10204=ORIENTED_EDGE('',*,*,#8015,.T.);
#10205=ORIENTED_EDGE('',*,*,#8019,.T.);
#10206=ORIENTED_EDGE('',*,*,#8038,.F.);
#10207=ORIENTED_EDGE('',*,*,#8039,.T.);
#10208=ORIENTED_EDGE('',*,*,#8040,.F.);
#10209=ORIENTED_EDGE('',*,*,#8041,.F.);
#10210=ORIENTED_EDGE('',*,*,#8042,.T.);
#10211=ORIENTED_EDGE('',*,*,#8043,.F.);
#10212=ORIENTED_EDGE('',*,*,#8042,.F.);
#10213=ORIENTED_EDGE('',*,*,#8044,.F.);
#10214=ORIENTED_EDGE('',*,*,#8045,.F.);
#10215=ORIENTED_EDGE('',*,*,#8039,.F.);
#10216=ORIENTED_EDGE('',*,*,#8046,.F.);
#10217=ORIENTED_EDGE('',*,*,#8044,.T.);
#10218=ORIENTED_EDGE('',*,*,#8041,.T.);
#10219=ORIENTED_EDGE('',*,*,#8047,.F.);
#10220=ORIENTED_EDGE('',*,*,#8048,.T.);
#10221=ORIENTED_EDGE('',*,*,#8049,.F.);
#10222=ORIENTED_EDGE('',*,*,#8048,.F.);
#10223=ORIENTED_EDGE('',*,*,#8045,.T.);
#10224=ORIENTED_EDGE('',*,*,#8046,.T.);
#10225=ORIENTED_EDGE('',*,*,#8040,.T.);
#10226=ORIENTED_EDGE('',*,*,#8038,.T.);
#10227=ORIENTED_EDGE('',*,*,#8050,.T.);
#10228=ORIENTED_EDGE('',*,*,#8051,.T.);
#10229=ORIENTED_EDGE('',*,*,#8052,.F.);
#10230=ORIENTED_EDGE('',*,*,#8053,.F.);
#10231=ORIENTED_EDGE('',*,*,#8049,.T.);
#10232=ORIENTED_EDGE('',*,*,#8054,.T.);
#10233=ORIENTED_EDGE('',*,*,#8053,.T.);
#10234=ORIENTED_EDGE('',*,*,#8055,.F.);
#10235=ORIENTED_EDGE('',*,*,#8056,.F.);
#10236=ORIENTED_EDGE('',*,*,#8043,.T.);
#10237=ORIENTED_EDGE('',*,*,#8057,.T.);
#10238=ORIENTED_EDGE('',*,*,#8056,.T.);
#10239=ORIENTED_EDGE('',*,*,#8058,.F.);
#10240=ORIENTED_EDGE('',*,*,#8059,.F.);
#10241=ORIENTED_EDGE('',*,*,#8047,.T.);
#10242=ORIENTED_EDGE('',*,*,#8060,.T.);
#10243=ORIENTED_EDGE('',*,*,#8059,.T.);
#10244=ORIENTED_EDGE('',*,*,#8061,.F.);
#10245=ORIENTED_EDGE('',*,*,#8051,.F.);
#10246=ORIENTED_EDGE('',*,*,#8061,.T.);
#10247=ORIENTED_EDGE('',*,*,#8058,.T.);
#10248=ORIENTED_EDGE('',*,*,#8055,.T.);
#10249=ORIENTED_EDGE('',*,*,#8052,.T.);
#10250=ORIENTED_EDGE('',*,*,#8060,.F.);
#10251=ORIENTED_EDGE('',*,*,#8050,.F.);
#10252=ORIENTED_EDGE('',*,*,#8054,.F.);
#10253=ORIENTED_EDGE('',*,*,#8057,.F.);
#10254=ORIENTED_EDGE('',*,*,#8062,.F.);
#10255=ORIENTED_EDGE('',*,*,#8063,.T.);
#10256=ORIENTED_EDGE('',*,*,#8064,.F.);
#10257=ORIENTED_EDGE('',*,*,#8063,.F.);
#10258=ORIENTED_EDGE('',*,*,#8062,.T.);
#10259=ORIENTED_EDGE('',*,*,#8065,.F.);
#10260=ORIENTED_EDGE('',*,*,#8066,.T.);
#10261=ORIENTED_EDGE('',*,*,#8067,.T.);
#10262=ORIENTED_EDGE('',*,*,#8066,.F.);
#10263=ORIENTED_EDGE('',*,*,#8067,.F.);
#10264=ORIENTED_EDGE('',*,*,#8068,.F.);
#10265=ORIENTED_EDGE('',*,*,#8069,.T.);
#10266=ORIENTED_EDGE('',*,*,#8070,.T.);
#10267=ORIENTED_EDGE('',*,*,#8069,.F.);
#10268=ORIENTED_EDGE('',*,*,#8068,.T.);
#10269=ORIENTED_EDGE('',*,*,#8064,.T.);
#10270=ORIENTED_EDGE('',*,*,#8070,.F.);
#10271=ORIENTED_EDGE('',*,*,#8065,.T.);
#10272=ORIENTED_EDGE('',*,*,#8071,.F.);
#10273=ORIENTED_EDGE('',*,*,#8072,.T.);
#10274=ORIENTED_EDGE('',*,*,#8073,.T.);
#10275=ORIENTED_EDGE('',*,*,#8072,.F.);
#10276=ORIENTED_EDGE('',*,*,#8074,.F.);
#10277=ORIENTED_EDGE('',*,*,#8075,.T.);
#10278=ORIENTED_EDGE('',*,*,#8076,.T.);
#10279=ORIENTED_EDGE('',*,*,#8075,.F.);
#10280=ORIENTED_EDGE('',*,*,#8074,.T.);
#10281=ORIENTED_EDGE('',*,*,#8071,.T.);
#10282=ORIENTED_EDGE('',*,*,#8076,.F.);
#10283=ORIENTED_EDGE('',*,*,#8073,.F.);
#10284=ORIENTED_EDGE('',*,*,#8077,.F.);
#10285=ORIENTED_EDGE('',*,*,#8078,.T.);
#10286=ORIENTED_EDGE('',*,*,#8079,.T.);
#10287=ORIENTED_EDGE('',*,*,#8078,.F.);
#10288=ORIENTED_EDGE('',*,*,#8080,.F.);
#10289=ORIENTED_EDGE('',*,*,#8081,.T.);
#10290=ORIENTED_EDGE('',*,*,#8082,.T.);
#10291=ORIENTED_EDGE('',*,*,#8081,.F.);
#10292=ORIENTED_EDGE('',*,*,#8080,.T.);
#10293=ORIENTED_EDGE('',*,*,#8077,.T.);
#10294=ORIENTED_EDGE('',*,*,#8082,.F.);
#10295=ORIENTED_EDGE('',*,*,#8079,.F.);
#10296=ORIENTED_EDGE('',*,*,#8083,.F.);
#10297=ORIENTED_EDGE('',*,*,#8084,.T.);
#10298=ORIENTED_EDGE('',*,*,#8085,.T.);
#10299=ORIENTED_EDGE('',*,*,#8084,.F.);
#10300=ORIENTED_EDGE('',*,*,#8086,.F.);
#10301=ORIENTED_EDGE('',*,*,#8087,.T.);
#10302=ORIENTED_EDGE('',*,*,#8088,.T.);
#10303=ORIENTED_EDGE('',*,*,#8087,.F.);
#10304=ORIENTED_EDGE('',*,*,#8086,.T.);
#10305=ORIENTED_EDGE('',*,*,#8083,.T.);
#10306=ORIENTED_EDGE('',*,*,#8088,.F.);
#10307=ORIENTED_EDGE('',*,*,#8085,.F.);
#10308=ORIENTED_EDGE('',*,*,#8089,.F.);
#10309=ORIENTED_EDGE('',*,*,#8090,.T.);
#10310=ORIENTED_EDGE('',*,*,#8091,.T.);
#10311=ORIENTED_EDGE('',*,*,#8090,.F.);
#10312=ORIENTED_EDGE('',*,*,#8092,.F.);
#10313=ORIENTED_EDGE('',*,*,#8093,.T.);
#10314=ORIENTED_EDGE('',*,*,#8094,.T.);
#10315=ORIENTED_EDGE('',*,*,#8093,.F.);
#10316=ORIENTED_EDGE('',*,*,#8092,.T.);
#10317=ORIENTED_EDGE('',*,*,#8089,.T.);
#10318=ORIENTED_EDGE('',*,*,#8094,.F.);
#10319=ORIENTED_EDGE('',*,*,#8091,.F.);
#10320=ORIENTED_EDGE('',*,*,#8095,.F.);
#10321=ORIENTED_EDGE('',*,*,#8096,.T.);
#10322=ORIENTED_EDGE('',*,*,#8097,.T.);
#10323=ORIENTED_EDGE('',*,*,#8096,.F.);
#10324=ORIENTED_EDGE('',*,*,#8098,.F.);
#10325=ORIENTED_EDGE('',*,*,#8099,.T.);
#10326=ORIENTED_EDGE('',*,*,#8100,.T.);
#10327=ORIENTED_EDGE('',*,*,#8099,.F.);
#10328=ORIENTED_EDGE('',*,*,#8098,.T.);
#10329=ORIENTED_EDGE('',*,*,#8095,.T.);
#10330=ORIENTED_EDGE('',*,*,#8100,.F.);
#10331=ORIENTED_EDGE('',*,*,#8097,.F.);
#10332=ORIENTED_EDGE('',*,*,#8101,.F.);
#10333=ORIENTED_EDGE('',*,*,#8102,.T.);
#10334=ORIENTED_EDGE('',*,*,#8103,.T.);
#10335=ORIENTED_EDGE('',*,*,#8102,.F.);
#10336=ORIENTED_EDGE('',*,*,#8104,.F.);
#10337=ORIENTED_EDGE('',*,*,#8105,.T.);
#10338=ORIENTED_EDGE('',*,*,#8106,.T.);
#10339=ORIENTED_EDGE('',*,*,#8105,.F.);
#10340=ORIENTED_EDGE('',*,*,#8104,.T.);
#10341=ORIENTED_EDGE('',*,*,#8101,.T.);
#10342=ORIENTED_EDGE('',*,*,#8106,.F.);
#10343=ORIENTED_EDGE('',*,*,#8103,.F.);
#10344=ORIENTED_EDGE('',*,*,#8107,.F.);
#10345=ORIENTED_EDGE('',*,*,#8108,.T.);
#10346=ORIENTED_EDGE('',*,*,#8109,.F.);
#10347=ORIENTED_EDGE('',*,*,#8108,.F.);
#10348=ORIENTED_EDGE('',*,*,#8110,.F.);
#10349=ORIENTED_EDGE('',*,*,#8111,.T.);
#10350=ORIENTED_EDGE('',*,*,#8112,.F.);
#10351=ORIENTED_EDGE('',*,*,#8111,.F.);
#10352=ORIENTED_EDGE('',*,*,#8113,.F.);
#10353=ORIENTED_EDGE('',*,*,#8114,.T.);
#10354=ORIENTED_EDGE('',*,*,#8115,.F.);
#10355=ORIENTED_EDGE('',*,*,#8114,.F.);
#10356=ORIENTED_EDGE('',*,*,#8116,.T.);
#10357=ORIENTED_EDGE('',*,*,#8117,.T.);
#10358=ORIENTED_EDGE('',*,*,#8118,.F.);
#10359=ORIENTED_EDGE('',*,*,#8119,.F.);
#10360=ORIENTED_EDGE('',*,*,#8120,.T.);
#10361=ORIENTED_EDGE('',*,*,#8119,.T.);
#10362=ORIENTED_EDGE('',*,*,#8121,.F.);
#10363=ORIENTED_EDGE('',*,*,#8122,.F.);
#10364=ORIENTED_EDGE('',*,*,#8109,.T.);
#10365=ORIENTED_EDGE('',*,*,#8112,.T.);
#10366=ORIENTED_EDGE('',*,*,#8115,.T.);
#10367=ORIENTED_EDGE('',*,*,#8123,.T.);
#10368=ORIENTED_EDGE('',*,*,#8122,.T.);
#10369=ORIENTED_EDGE('',*,*,#8124,.F.);
#10370=ORIENTED_EDGE('',*,*,#8125,.F.);
#10371=ORIENTED_EDGE('',*,*,#8126,.T.);
#10372=ORIENTED_EDGE('',*,*,#8125,.T.);
#10373=ORIENTED_EDGE('',*,*,#8127,.F.);
#10374=ORIENTED_EDGE('',*,*,#8117,.F.);
#10375=ORIENTED_EDGE('',*,*,#8107,.T.);
#10376=ORIENTED_EDGE('',*,*,#8110,.T.);
#10377=ORIENTED_EDGE('',*,*,#8113,.T.);
#10378=ORIENTED_EDGE('',*,*,#8127,.T.);
#10379=ORIENTED_EDGE('',*,*,#8124,.T.);
#10380=ORIENTED_EDGE('',*,*,#8121,.T.);
#10381=ORIENTED_EDGE('',*,*,#8118,.T.);
#10382=ORIENTED_EDGE('',*,*,#8126,.F.);
#10383=ORIENTED_EDGE('',*,*,#8116,.F.);
#10384=ORIENTED_EDGE('',*,*,#8120,.F.);
#10385=ORIENTED_EDGE('',*,*,#8123,.F.);
#10386=ORIENTED_EDGE('',*,*,#8128,.F.);
#10387=ORIENTED_EDGE('',*,*,#8129,.T.);
#10388=ORIENTED_EDGE('',*,*,#8130,.F.);
#10389=ORIENTED_EDGE('',*,*,#8129,.F.);
#10390=ORIENTED_EDGE('',*,*,#8128,.T.);
#10391=ORIENTED_EDGE('',*,*,#8131,.T.);
#10392=ORIENTED_EDGE('',*,*,#8132,.F.);
#10393=ORIENTED_EDGE('',*,*,#8133,.T.);
#10394=ORIENTED_EDGE('',*,*,#8134,.F.);
#10395=ORIENTED_EDGE('',*,*,#8133,.F.);
#10396=ORIENTED_EDGE('',*,*,#8132,.T.);
#10397=ORIENTED_EDGE('',*,*,#8135,.T.);
#10398=ORIENTED_EDGE('',*,*,#8136,.F.);
#10399=ORIENTED_EDGE('',*,*,#8137,.T.);
#10400=ORIENTED_EDGE('',*,*,#8138,.F.);
#10401=ORIENTED_EDGE('',*,*,#8137,.F.);
#10402=ORIENTED_EDGE('',*,*,#8139,.F.);
#10403=ORIENTED_EDGE('',*,*,#8140,.T.);
#10404=ORIENTED_EDGE('',*,*,#8135,.F.);
#10405=ORIENTED_EDGE('',*,*,#8140,.F.);
#10406=ORIENTED_EDGE('',*,*,#8141,.F.);
#10407=ORIENTED_EDGE('',*,*,#8142,.T.);
#10408=ORIENTED_EDGE('',*,*,#8131,.F.);
#10409=ORIENTED_EDGE('',*,*,#8142,.F.);
#10410=ORIENTED_EDGE('',*,*,#8143,.T.);
#10411=ORIENTED_EDGE('',*,*,#8144,.T.);
#10412=ORIENTED_EDGE('',*,*,#8145,.F.);
#10413=ORIENTED_EDGE('',*,*,#8146,.F.);
#10414=ORIENTED_EDGE('',*,*,#8147,.T.);
#10415=ORIENTED_EDGE('',*,*,#8146,.T.);
#10416=ORIENTED_EDGE('',*,*,#8148,.F.);
#10417=ORIENTED_EDGE('',*,*,#8149,.F.);
#10418=ORIENTED_EDGE('',*,*,#8150,.T.);
#10419=ORIENTED_EDGE('',*,*,#8149,.T.);
#10420=ORIENTED_EDGE('',*,*,#8151,.F.);
#10421=ORIENTED_EDGE('',*,*,#8152,.F.);
#10422=ORIENTED_EDGE('',*,*,#8153,.T.);
#10423=ORIENTED_EDGE('',*,*,#8152,.T.);
#10424=ORIENTED_EDGE('',*,*,#8154,.F.);
#10425=ORIENTED_EDGE('',*,*,#8144,.F.);
#10426=ORIENTED_EDGE('',*,*,#8154,.T.);
#10427=ORIENTED_EDGE('',*,*,#8151,.T.);
#10428=ORIENTED_EDGE('',*,*,#8148,.T.);
#10429=ORIENTED_EDGE('',*,*,#8145,.T.);
#10430=ORIENTED_EDGE('',*,*,#8130,.T.);
#10431=ORIENTED_EDGE('',*,*,#8134,.T.);
#10432=ORIENTED_EDGE('',*,*,#8138,.T.);
#10433=ORIENTED_EDGE('',*,*,#8153,.F.);
#10434=ORIENTED_EDGE('',*,*,#8143,.F.);
#10435=ORIENTED_EDGE('',*,*,#8147,.F.);
#10436=ORIENTED_EDGE('',*,*,#8150,.F.);
#10437=ORIENTED_EDGE('',*,*,#8136,.T.);
#10438=ORIENTED_EDGE('',*,*,#8139,.T.);
#10439=ORIENTED_EDGE('',*,*,#8141,.T.);
#10440=ORIENTED_EDGE('',*,*,#8155,.F.);
#10441=ORIENTED_EDGE('',*,*,#8156,.T.);
#10442=ORIENTED_EDGE('',*,*,#8157,.T.);
#10443=ORIENTED_EDGE('',*,*,#8156,.F.);
#10444=ORIENTED_EDGE('',*,*,#8157,.F.);
#10445=ORIENTED_EDGE('',*,*,#8158,.F.);
#10446=ORIENTED_EDGE('',*,*,#8159,.F.);
#10447=ORIENTED_EDGE('',*,*,#8160,.T.);
#10448=ORIENTED_EDGE('',*,*,#8161,.T.);
#10449=ORIENTED_EDGE('',*,*,#8160,.F.);
#10450=ORIENTED_EDGE('',*,*,#8161,.F.);
#10451=ORIENTED_EDGE('',*,*,#8162,.F.);
#10452=ORIENTED_EDGE('',*,*,#8163,.F.);
#10453=ORIENTED_EDGE('',*,*,#8164,.T.);
#10454=ORIENTED_EDGE('',*,*,#8165,.F.);
#10455=ORIENTED_EDGE('',*,*,#8164,.F.);
#10456=ORIENTED_EDGE('',*,*,#8162,.T.);
#10457=ORIENTED_EDGE('',*,*,#8166,.T.);
#10458=ORIENTED_EDGE('',*,*,#8167,.F.);
#10459=ORIENTED_EDGE('',*,*,#8166,.F.);
#10460=ORIENTED_EDGE('',*,*,#8158,.T.);
#10461=ORIENTED_EDGE('',*,*,#8168,.T.);
#10462=ORIENTED_EDGE('',*,*,#8169,.F.);
#10463=ORIENTED_EDGE('',*,*,#8168,.F.);
#10464=ORIENTED_EDGE('',*,*,#8170,.T.);
#10465=ORIENTED_EDGE('',*,*,#8171,.T.);
#10466=ORIENTED_EDGE('',*,*,#8172,.F.);
#10467=ORIENTED_EDGE('',*,*,#8173,.F.);
#10468=ORIENTED_EDGE('',*,*,#8174,.T.);
#10469=ORIENTED_EDGE('',*,*,#8173,.T.);
#10470=ORIENTED_EDGE('',*,*,#8175,.F.);
#10471=ORIENTED_EDGE('',*,*,#8176,.F.);
#10472=ORIENTED_EDGE('',*,*,#8177,.T.);
#10473=ORIENTED_EDGE('',*,*,#8176,.T.);
#10474=ORIENTED_EDGE('',*,*,#8178,.F.);
#10475=ORIENTED_EDGE('',*,*,#8179,.F.);
#10476=ORIENTED_EDGE('',*,*,#8180,.T.);
#10477=ORIENTED_EDGE('',*,*,#8179,.T.);
#10478=ORIENTED_EDGE('',*,*,#8181,.F.);
#10479=ORIENTED_EDGE('',*,*,#8171,.F.);
#10480=ORIENTED_EDGE('',*,*,#8181,.T.);
#10481=ORIENTED_EDGE('',*,*,#8178,.T.);
#10482=ORIENTED_EDGE('',*,*,#8175,.T.);
#10483=ORIENTED_EDGE('',*,*,#8172,.T.);
#10484=ORIENTED_EDGE('',*,*,#8165,.T.);
#10485=ORIENTED_EDGE('',*,*,#8167,.T.);
#10486=ORIENTED_EDGE('',*,*,#8169,.T.);
#10487=ORIENTED_EDGE('',*,*,#8180,.F.);
#10488=ORIENTED_EDGE('',*,*,#8170,.F.);
#10489=ORIENTED_EDGE('',*,*,#8174,.F.);
#10490=ORIENTED_EDGE('',*,*,#8177,.F.);
#10491=ORIENTED_EDGE('',*,*,#8155,.T.);
#10492=ORIENTED_EDGE('',*,*,#8159,.T.);
#10493=ORIENTED_EDGE('',*,*,#8163,.T.);
#10494=ORIENTED_EDGE('',*,*,#8182,.F.);
#10495=ORIENTED_EDGE('',*,*,#8183,.T.);
#10496=ORIENTED_EDGE('',*,*,#8184,.F.);
#10497=ORIENTED_EDGE('',*,*,#8185,.F.);
#10498=ORIENTED_EDGE('',*,*,#8186,.T.);
#10499=ORIENTED_EDGE('',*,*,#8187,.F.);
#10500=ORIENTED_EDGE('',*,*,#8186,.F.);
#10501=ORIENTED_EDGE('',*,*,#8188,.F.);
#10502=ORIENTED_EDGE('',*,*,#8189,.F.);
#10503=ORIENTED_EDGE('',*,*,#8183,.F.);
#10504=ORIENTED_EDGE('',*,*,#8190,.F.);
#10505=ORIENTED_EDGE('',*,*,#8188,.T.);
#10506=ORIENTED_EDGE('',*,*,#8185,.T.);
#10507=ORIENTED_EDGE('',*,*,#8191,.F.);
#10508=ORIENTED_EDGE('',*,*,#8192,.T.);
#10509=ORIENTED_EDGE('',*,*,#8193,.F.);
#10510=ORIENTED_EDGE('',*,*,#8192,.F.);
#10511=ORIENTED_EDGE('',*,*,#8189,.T.);
#10512=ORIENTED_EDGE('',*,*,#8190,.T.);
#10513=ORIENTED_EDGE('',*,*,#8184,.T.);
#10514=ORIENTED_EDGE('',*,*,#8182,.T.);
#10515=ORIENTED_EDGE('',*,*,#8194,.T.);
#10516=ORIENTED_EDGE('',*,*,#8195,.T.);
#10517=ORIENTED_EDGE('',*,*,#8196,.F.);
#10518=ORIENTED_EDGE('',*,*,#8197,.F.);
#10519=ORIENTED_EDGE('',*,*,#8193,.T.);
#10520=ORIENTED_EDGE('',*,*,#8198,.T.);
#10521=ORIENTED_EDGE('',*,*,#8197,.T.);
#10522=ORIENTED_EDGE('',*,*,#8199,.F.);
#10523=ORIENTED_EDGE('',*,*,#8200,.F.);
#10524=ORIENTED_EDGE('',*,*,#8187,.T.);
#10525=ORIENTED_EDGE('',*,*,#8201,.T.);
#10526=ORIENTED_EDGE('',*,*,#8200,.T.);
#10527=ORIENTED_EDGE('',*,*,#8202,.F.);
#10528=ORIENTED_EDGE('',*,*,#8203,.F.);
#10529=ORIENTED_EDGE('',*,*,#8191,.T.);
#10530=ORIENTED_EDGE('',*,*,#8204,.T.);
#10531=ORIENTED_EDGE('',*,*,#8203,.T.);
#10532=ORIENTED_EDGE('',*,*,#8205,.F.);
#10533=ORIENTED_EDGE('',*,*,#8195,.F.);
#10534=ORIENTED_EDGE('',*,*,#8205,.T.);
#10535=ORIENTED_EDGE('',*,*,#8202,.T.);
#10536=ORIENTED_EDGE('',*,*,#8199,.T.);
#10537=ORIENTED_EDGE('',*,*,#8196,.T.);
#10538=ORIENTED_EDGE('',*,*,#8204,.F.);
#10539=ORIENTED_EDGE('',*,*,#8194,.F.);
#10540=ORIENTED_EDGE('',*,*,#8198,.F.);
#10541=ORIENTED_EDGE('',*,*,#8201,.F.);
#10542=ORIENTED_EDGE('',*,*,#8206,.F.);
#10543=ORIENTED_EDGE('',*,*,#8207,.T.);
#10544=ORIENTED_EDGE('',*,*,#8208,.F.);
#10545=ORIENTED_EDGE('',*,*,#8207,.F.);
#10546=ORIENTED_EDGE('',*,*,#8206,.T.);
#10547=ORIENTED_EDGE('',*,*,#8209,.F.);
#10548=ORIENTED_EDGE('',*,*,#8210,.T.);
#10549=ORIENTED_EDGE('',*,*,#8211,.T.);
#10550=ORIENTED_EDGE('',*,*,#8210,.F.);
#10551=ORIENTED_EDGE('',*,*,#8211,.F.);
#10552=ORIENTED_EDGE('',*,*,#8212,.F.);
#10553=ORIENTED_EDGE('',*,*,#8213,.T.);
#10554=ORIENTED_EDGE('',*,*,#8214,.T.);
#10555=ORIENTED_EDGE('',*,*,#8213,.F.);
#10556=ORIENTED_EDGE('',*,*,#8212,.T.);
#10557=ORIENTED_EDGE('',*,*,#8208,.T.);
#10558=ORIENTED_EDGE('',*,*,#8214,.F.);
#10559=ORIENTED_EDGE('',*,*,#8209,.T.);
#10560=ORIENTED_EDGE('',*,*,#8215,.F.);
#10561=ORIENTED_EDGE('',*,*,#8216,.T.);
#10562=ORIENTED_EDGE('',*,*,#8217,.T.);
#10563=ORIENTED_EDGE('',*,*,#8216,.F.);
#10564=ORIENTED_EDGE('',*,*,#8218,.F.);
#10565=ORIENTED_EDGE('',*,*,#8219,.T.);
#10566=ORIENTED_EDGE('',*,*,#8220,.T.);
#10567=ORIENTED_EDGE('',*,*,#8219,.F.);
#10568=ORIENTED_EDGE('',*,*,#8218,.T.);
#10569=ORIENTED_EDGE('',*,*,#8215,.T.);
#10570=ORIENTED_EDGE('',*,*,#8220,.F.);
#10571=ORIENTED_EDGE('',*,*,#8217,.F.);
#10572=ORIENTED_EDGE('',*,*,#8221,.F.);
#10573=ORIENTED_EDGE('',*,*,#8222,.T.);
#10574=ORIENTED_EDGE('',*,*,#8223,.T.);
#10575=ORIENTED_EDGE('',*,*,#8222,.F.);
#10576=ORIENTED_EDGE('',*,*,#8224,.F.);
#10577=ORIENTED_EDGE('',*,*,#8225,.T.);
#10578=ORIENTED_EDGE('',*,*,#8226,.T.);
#10579=ORIENTED_EDGE('',*,*,#8225,.F.);
#10580=ORIENTED_EDGE('',*,*,#8224,.T.);
#10581=ORIENTED_EDGE('',*,*,#8221,.T.);
#10582=ORIENTED_EDGE('',*,*,#8226,.F.);
#10583=ORIENTED_EDGE('',*,*,#8223,.F.);
#10584=ORIENTED_EDGE('',*,*,#8227,.F.);
#10585=ORIENTED_EDGE('',*,*,#8228,.T.);
#10586=ORIENTED_EDGE('',*,*,#8229,.T.);
#10587=ORIENTED_EDGE('',*,*,#8228,.F.);
#10588=ORIENTED_EDGE('',*,*,#8230,.F.);
#10589=ORIENTED_EDGE('',*,*,#8231,.T.);
#10590=ORIENTED_EDGE('',*,*,#8232,.T.);
#10591=ORIENTED_EDGE('',*,*,#8231,.F.);
#10592=ORIENTED_EDGE('',*,*,#8230,.T.);
#10593=ORIENTED_EDGE('',*,*,#8227,.T.);
#10594=ORIENTED_EDGE('',*,*,#8232,.F.);
#10595=ORIENTED_EDGE('',*,*,#8229,.F.);
#10596=ORIENTED_EDGE('',*,*,#8233,.F.);
#10597=ORIENTED_EDGE('',*,*,#8234,.T.);
#10598=ORIENTED_EDGE('',*,*,#8235,.T.);
#10599=ORIENTED_EDGE('',*,*,#8234,.F.);
#10600=ORIENTED_EDGE('',*,*,#8236,.F.);
#10601=ORIENTED_EDGE('',*,*,#8237,.T.);
#10602=ORIENTED_EDGE('',*,*,#8238,.T.);
#10603=ORIENTED_EDGE('',*,*,#8237,.F.);
#10604=ORIENTED_EDGE('',*,*,#8236,.T.);
#10605=ORIENTED_EDGE('',*,*,#8233,.T.);
#10606=ORIENTED_EDGE('',*,*,#8238,.F.);
#10607=ORIENTED_EDGE('',*,*,#8235,.F.);
#10608=ORIENTED_EDGE('',*,*,#8239,.F.);
#10609=ORIENTED_EDGE('',*,*,#8240,.T.);
#10610=ORIENTED_EDGE('',*,*,#8241,.T.);
#10611=ORIENTED_EDGE('',*,*,#8240,.F.);
#10612=ORIENTED_EDGE('',*,*,#8242,.F.);
#10613=ORIENTED_EDGE('',*,*,#8243,.T.);
#10614=ORIENTED_EDGE('',*,*,#8244,.T.);
#10615=ORIENTED_EDGE('',*,*,#8243,.F.);
#10616=ORIENTED_EDGE('',*,*,#8242,.T.);
#10617=ORIENTED_EDGE('',*,*,#8239,.T.);
#10618=ORIENTED_EDGE('',*,*,#8244,.F.);
#10619=ORIENTED_EDGE('',*,*,#8241,.F.);
#10620=ORIENTED_EDGE('',*,*,#8245,.F.);
#10621=ORIENTED_EDGE('',*,*,#8246,.T.);
#10622=ORIENTED_EDGE('',*,*,#8247,.T.);
#10623=ORIENTED_EDGE('',*,*,#8246,.F.);
#10624=ORIENTED_EDGE('',*,*,#8248,.F.);
#10625=ORIENTED_EDGE('',*,*,#8249,.T.);
#10626=ORIENTED_EDGE('',*,*,#8250,.T.);
#10627=ORIENTED_EDGE('',*,*,#8249,.F.);
#10628=ORIENTED_EDGE('',*,*,#8248,.T.);
#10629=ORIENTED_EDGE('',*,*,#8245,.T.);
#10630=ORIENTED_EDGE('',*,*,#8250,.F.);
#10631=ORIENTED_EDGE('',*,*,#8247,.F.);
#10632=ORIENTED_EDGE('',*,*,#8251,.F.);
#10633=ORIENTED_EDGE('',*,*,#8252,.F.);
#10634=ORIENTED_EDGE('',*,*,#8253,.F.);
#10635=ORIENTED_EDGE('',*,*,#8254,.F.);
#10636=ORIENTED_EDGE('',*,*,#8255,.F.);
#10637=ORIENTED_EDGE('',*,*,#8254,.T.);
#10638=ORIENTED_EDGE('',*,*,#8256,.F.);
#10639=ORIENTED_EDGE('',*,*,#8257,.T.);
#10640=ORIENTED_EDGE('',*,*,#8258,.F.);
#10641=ORIENTED_EDGE('',*,*,#8257,.F.);
#10642=ORIENTED_EDGE('',*,*,#8259,.F.);
#10643=ORIENTED_EDGE('',*,*,#8260,.F.);
#10644=ORIENTED_EDGE('',*,*,#8261,.F.);
#10645=ORIENTED_EDGE('',*,*,#8260,.T.);
#10646=ORIENTED_EDGE('',*,*,#8262,.T.);
#10647=ORIENTED_EDGE('',*,*,#8252,.T.);
#10648=ORIENTED_EDGE('',*,*,#8262,.F.);
#10649=ORIENTED_EDGE('',*,*,#8259,.T.);
#10650=ORIENTED_EDGE('',*,*,#8256,.T.);
#10651=ORIENTED_EDGE('',*,*,#8253,.T.);
#10652=ORIENTED_EDGE('',*,*,#8263,.F.);
#10653=ORIENTED_EDGE('',*,*,#8264,.T.);
#10654=ORIENTED_EDGE('',*,*,#8265,.F.);
#10655=ORIENTED_EDGE('',*,*,#8266,.T.);
#10656=ORIENTED_EDGE('',*,*,#8263,.T.);
#10657=ORIENTED_EDGE('',*,*,#8266,.F.);
#10658=ORIENTED_EDGE('',*,*,#8265,.T.);
#10659=ORIENTED_EDGE('',*,*,#8267,.F.);
#10660=ORIENTED_EDGE('',*,*,#8268,.F.);
#10661=ORIENTED_EDGE('',*,*,#8269,.T.);
#10662=ORIENTED_EDGE('',*,*,#8267,.T.);
#10663=ORIENTED_EDGE('',*,*,#8269,.F.);
#10664=ORIENTED_EDGE('',*,*,#8270,.F.);
#10665=ORIENTED_EDGE('',*,*,#8268,.T.);
#10666=ORIENTED_EDGE('',*,*,#8271,.F.);
#10667=ORIENTED_EDGE('',*,*,#8272,.T.);
#10668=ORIENTED_EDGE('',*,*,#8270,.T.);
#10669=ORIENTED_EDGE('',*,*,#8272,.F.);
#10670=ORIENTED_EDGE('',*,*,#8271,.T.);
#10671=ORIENTED_EDGE('',*,*,#8273,.F.);
#10672=ORIENTED_EDGE('',*,*,#8274,.F.);
#10673=ORIENTED_EDGE('',*,*,#8275,.T.);
#10674=ORIENTED_EDGE('',*,*,#8273,.T.);
#10675=ORIENTED_EDGE('',*,*,#8275,.F.);
#10676=ORIENTED_EDGE('',*,*,#8276,.F.);
#10677=ORIENTED_EDGE('',*,*,#8274,.T.);
#10678=ORIENTED_EDGE('',*,*,#8277,.F.);
#10679=ORIENTED_EDGE('',*,*,#8278,.T.);
#10680=ORIENTED_EDGE('',*,*,#8276,.T.);
#10681=ORIENTED_EDGE('',*,*,#8278,.F.);
#10682=ORIENTED_EDGE('',*,*,#8277,.T.);
#10683=ORIENTED_EDGE('',*,*,#8279,.F.);
#10684=ORIENTED_EDGE('',*,*,#8279,.T.);
#10685=ORIENTED_EDGE('',*,*,#8280,.T.);
#10686=ORIENTED_EDGE('',*,*,#8264,.F.);
#10687=ORIENTED_EDGE('',*,*,#8280,.F.);
#10688=ORIENTED_EDGE('',*,*,#8258,.T.);
#10689=ORIENTED_EDGE('',*,*,#8261,.T.);
#10690=ORIENTED_EDGE('',*,*,#8251,.T.);
#10691=ORIENTED_EDGE('',*,*,#8255,.T.);
#10692=ORIENTED_EDGE('',*,*,#8281,.F.);
#10693=ORIENTED_EDGE('',*,*,#8282,.F.);
#10694=ORIENTED_EDGE('',*,*,#8283,.F.);
#10695=ORIENTED_EDGE('',*,*,#8284,.F.);
#10696=ORIENTED_EDGE('',*,*,#8285,.F.);
#10697=ORIENTED_EDGE('',*,*,#8284,.T.);
#10698=ORIENTED_EDGE('',*,*,#8286,.F.);
#10699=ORIENTED_EDGE('',*,*,#8287,.T.);
#10700=ORIENTED_EDGE('',*,*,#8288,.F.);
#10701=ORIENTED_EDGE('',*,*,#8287,.F.);
#10702=ORIENTED_EDGE('',*,*,#8289,.F.);
#10703=ORIENTED_EDGE('',*,*,#8290,.F.);
#10704=ORIENTED_EDGE('',*,*,#8291,.F.);
#10705=ORIENTED_EDGE('',*,*,#8290,.T.);
#10706=ORIENTED_EDGE('',*,*,#8292,.F.);
#10707=ORIENTED_EDGE('',*,*,#8282,.T.);
#10708=ORIENTED_EDGE('',*,*,#8293,.F.);
#10709=ORIENTED_EDGE('',*,*,#8294,.T.);
#10710=ORIENTED_EDGE('',*,*,#8295,.F.);
#10711=ORIENTED_EDGE('',*,*,#8296,.T.);
#10712=ORIENTED_EDGE('',*,*,#8293,.T.);
#10713=ORIENTED_EDGE('',*,*,#8296,.F.);
#10714=ORIENTED_EDGE('',*,*,#8288,.T.);
#10715=ORIENTED_EDGE('',*,*,#8291,.T.);
#10716=ORIENTED_EDGE('',*,*,#8281,.T.);
#10717=ORIENTED_EDGE('',*,*,#8285,.T.);
#10718=ORIENTED_EDGE('',*,*,#8295,.T.);
#10719=ORIENTED_EDGE('',*,*,#8297,.F.);
#10720=ORIENTED_EDGE('',*,*,#8297,.T.);
#10721=ORIENTED_EDGE('',*,*,#8298,.T.);
#10722=ORIENTED_EDGE('',*,*,#8294,.F.);
#10723=ORIENTED_EDGE('',*,*,#8298,.F.);
#10724=ORIENTED_EDGE('',*,*,#8289,.T.);
#10725=ORIENTED_EDGE('',*,*,#8286,.T.);
#10726=ORIENTED_EDGE('',*,*,#8283,.T.);
#10727=ORIENTED_EDGE('',*,*,#8292,.T.);
#10728=ORIENTED_EDGE('',*,*,#8299,.F.);
#10729=ORIENTED_EDGE('',*,*,#8300,.F.);
#10730=ORIENTED_EDGE('',*,*,#8301,.T.);
#10731=ORIENTED_EDGE('',*,*,#8302,.T.);
#10732=ORIENTED_EDGE('',*,*,#8303,.F.);
#10733=ORIENTED_EDGE('',*,*,#8304,.F.);
#10734=ORIENTED_EDGE('',*,*,#8305,.T.);
#10735=ORIENTED_EDGE('',*,*,#8306,.T.);
#10736=ORIENTED_EDGE('',*,*,#8301,.F.);
#10737=ORIENTED_EDGE('',*,*,#8307,.F.);
#10738=ORIENTED_EDGE('',*,*,#8308,.T.);
#10739=ORIENTED_EDGE('',*,*,#8309,.T.);
#10740=ORIENTED_EDGE('',*,*,#8305,.F.);
#10741=ORIENTED_EDGE('',*,*,#8310,.F.);
#10742=ORIENTED_EDGE('',*,*,#8311,.T.);
#10743=ORIENTED_EDGE('',*,*,#8312,.T.);
#10744=ORIENTED_EDGE('',*,*,#8308,.F.);
#10745=ORIENTED_EDGE('',*,*,#8313,.F.);
#10746=ORIENTED_EDGE('',*,*,#8314,.T.);
#10747=ORIENTED_EDGE('',*,*,#8315,.T.);
#10748=ORIENTED_EDGE('',*,*,#8311,.F.);
#10749=ORIENTED_EDGE('',*,*,#8316,.F.);
#10750=ORIENTED_EDGE('',*,*,#8303,.T.);
#10751=ORIENTED_EDGE('',*,*,#8317,.T.);
#10752=ORIENTED_EDGE('',*,*,#8314,.F.);
#10753=ORIENTED_EDGE('',*,*,#8317,.F.);
#10754=ORIENTED_EDGE('',*,*,#8302,.F.);
#10755=ORIENTED_EDGE('',*,*,#8306,.F.);
#10756=ORIENTED_EDGE('',*,*,#8309,.F.);
#10757=ORIENTED_EDGE('',*,*,#8312,.F.);
#10758=ORIENTED_EDGE('',*,*,#8315,.F.);
#10759=ORIENTED_EDGE('',*,*,#8318,.F.);
#10760=ORIENTED_EDGE('',*,*,#8300,.T.);
#10761=ORIENTED_EDGE('',*,*,#8316,.T.);
#10762=ORIENTED_EDGE('',*,*,#8313,.T.);
#10763=ORIENTED_EDGE('',*,*,#8310,.T.);
#10764=ORIENTED_EDGE('',*,*,#8307,.T.);
#10765=ORIENTED_EDGE('',*,*,#8304,.T.);
#10766=ORIENTED_EDGE('',*,*,#8319,.F.);
#10767=ORIENTED_EDGE('',*,*,#8320,.T.);
#10768=ORIENTED_EDGE('',*,*,#8318,.T.);
#10769=ORIENTED_EDGE('',*,*,#8320,.F.);
#10770=ORIENTED_EDGE('',*,*,#8299,.T.);
#10771=ORIENTED_EDGE('',*,*,#8321,.T.);
#10772=ORIENTED_EDGE('',*,*,#8319,.T.);
#10773=ORIENTED_EDGE('',*,*,#8321,.F.);
#10774=ORIENTED_EDGE('',*,*,#8322,.F.);
#10775=ORIENTED_EDGE('',*,*,#8323,.T.);
#10776=ORIENTED_EDGE('',*,*,#8324,.F.);
#10777=ORIENTED_EDGE('',*,*,#8323,.F.);
#10778=ORIENTED_EDGE('',*,*,#8325,.F.);
#10779=ORIENTED_EDGE('',*,*,#8326,.T.);
#10780=ORIENTED_EDGE('',*,*,#8327,.F.);
#10781=ORIENTED_EDGE('',*,*,#8328,.F.);
#10782=ORIENTED_EDGE('',*,*,#8329,.F.);
#10783=ORIENTED_EDGE('',*,*,#8330,.F.);
#10784=ORIENTED_EDGE('',*,*,#8331,.F.);
#10785=ORIENTED_EDGE('',*,*,#8332,.T.);
#10786=ORIENTED_EDGE('',*,*,#8331,.T.);
#10787=ORIENTED_EDGE('',*,*,#8333,.F.);
#10788=ORIENTED_EDGE('',*,*,#8334,.T.);
#10789=ORIENTED_EDGE('',*,*,#8335,.T.);
#10790=ORIENTED_EDGE('',*,*,#8329,.T.);
#10791=ORIENTED_EDGE('',*,*,#8336,.T.);
#10792=ORIENTED_EDGE('',*,*,#8337,.T.);
#10793=ORIENTED_EDGE('',*,*,#8338,.F.);
#10794=ORIENTED_EDGE('',*,*,#8327,.T.);
#10795=ORIENTED_EDGE('',*,*,#8339,.T.);
#10796=ORIENTED_EDGE('',*,*,#8340,.T.);
#10797=ORIENTED_EDGE('',*,*,#8341,.F.);
#10798=ORIENTED_EDGE('',*,*,#8342,.F.);
#10799=ORIENTED_EDGE('',*,*,#8343,.T.);
#10800=ORIENTED_EDGE('',*,*,#8344,.F.);
#10801=ORIENTED_EDGE('',*,*,#8343,.F.);
#10802=ORIENTED_EDGE('',*,*,#8334,.F.);
#10803=ORIENTED_EDGE('',*,*,#8345,.F.);
#10804=ORIENTED_EDGE('',*,*,#8340,.F.);
#10805=ORIENTED_EDGE('',*,*,#8346,.T.);
#10806=ORIENTED_EDGE('',*,*,#8347,.F.);
#10807=ORIENTED_EDGE('',*,*,#8348,.F.);
#10808=ORIENTED_EDGE('',*,*,#8336,.F.);
#10809=ORIENTED_EDGE('',*,*,#8332,.F.);
#10810=ORIENTED_EDGE('',*,*,#8335,.F.);
#10811=ORIENTED_EDGE('',*,*,#8346,.F.);
#10812=ORIENTED_EDGE('',*,*,#8339,.F.);
#10813=ORIENTED_EDGE('',*,*,#8326,.F.);
#10814=ORIENTED_EDGE('',*,*,#8322,.T.);
#10815=ORIENTED_EDGE('',*,*,#8342,.T.);
#10816=ORIENTED_EDGE('',*,*,#8349,.T.);
#10817=ORIENTED_EDGE('',*,*,#8325,.T.);
#10818=ORIENTED_EDGE('',*,*,#8350,.F.);
#10819=ORIENTED_EDGE('',*,*,#8351,.T.);
#10820=ORIENTED_EDGE('',*,*,#8347,.T.);
#10821=ORIENTED_EDGE('',*,*,#8349,.F.);
#10822=ORIENTED_EDGE('',*,*,#8352,.T.);
#10823=ORIENTED_EDGE('',*,*,#8353,.F.);
#10824=ORIENTED_EDGE('',*,*,#8352,.F.);
#10825=ORIENTED_EDGE('',*,*,#8337,.F.);
#10826=ORIENTED_EDGE('',*,*,#8348,.T.);
#10827=ORIENTED_EDGE('',*,*,#8351,.F.);
#10828=ORIENTED_EDGE('',*,*,#8354,.F.);
#10829=ORIENTED_EDGE('',*,*,#8338,.T.);
#10830=ORIENTED_EDGE('',*,*,#8354,.T.);
#10831=ORIENTED_EDGE('',*,*,#8350,.T.);
#10832=ORIENTED_EDGE('',*,*,#8328,.T.);
#10833=ORIENTED_EDGE('',*,*,#8341,.T.);
#10834=ORIENTED_EDGE('',*,*,#8345,.T.);
#10835=ORIENTED_EDGE('',*,*,#8333,.T.);
#10836=ORIENTED_EDGE('',*,*,#8330,.T.);
#10837=ORIENTED_EDGE('',*,*,#8324,.T.);
#10838=ORIENTED_EDGE('',*,*,#8344,.T.);
#10839=ORIENTED_EDGE('',*,*,#8353,.T.);
#10840=ORIENTED_EDGE('',*,*,#8355,.F.);
#10841=ORIENTED_EDGE('',*,*,#8356,.T.);
#10842=ORIENTED_EDGE('',*,*,#8357,.T.);
#10843=ORIENTED_EDGE('',*,*,#8356,.F.);
#10844=ORIENTED_EDGE('',*,*,#8358,.F.);
#10845=ORIENTED_EDGE('',*,*,#8359,.T.);
#10846=ORIENTED_EDGE('',*,*,#8360,.T.);
#10847=ORIENTED_EDGE('',*,*,#8359,.F.);
#10848=ORIENTED_EDGE('',*,*,#8358,.T.);
#10849=ORIENTED_EDGE('',*,*,#8355,.T.);
#10850=ORIENTED_EDGE('',*,*,#8360,.F.);
#10851=ORIENTED_EDGE('',*,*,#8357,.F.);
#10852=ORIENTED_EDGE('',*,*,#8361,.F.);
#10853=ORIENTED_EDGE('',*,*,#8362,.T.);
#10854=ORIENTED_EDGE('',*,*,#8363,.T.);
#10855=ORIENTED_EDGE('',*,*,#8362,.F.);
#10856=ORIENTED_EDGE('',*,*,#8364,.F.);
#10857=ORIENTED_EDGE('',*,*,#8365,.T.);
#10858=ORIENTED_EDGE('',*,*,#8366,.T.);
#10859=ORIENTED_EDGE('',*,*,#8365,.F.);
#10860=ORIENTED_EDGE('',*,*,#8364,.T.);
#10861=ORIENTED_EDGE('',*,*,#8361,.T.);
#10862=ORIENTED_EDGE('',*,*,#8366,.F.);
#10863=ORIENTED_EDGE('',*,*,#8363,.F.);
#10864=ORIENTED_EDGE('',*,*,#8367,.F.);
#10865=ORIENTED_EDGE('',*,*,#8368,.T.);
#10866=ORIENTED_EDGE('',*,*,#8369,.T.);
#10867=ORIENTED_EDGE('',*,*,#8368,.F.);
#10868=ORIENTED_EDGE('',*,*,#8370,.F.);
#10869=ORIENTED_EDGE('',*,*,#8371,.T.);
#10870=ORIENTED_EDGE('',*,*,#8372,.T.);
#10871=ORIENTED_EDGE('',*,*,#8371,.F.);
#10872=ORIENTED_EDGE('',*,*,#8370,.T.);
#10873=ORIENTED_EDGE('',*,*,#8367,.T.);
#10874=ORIENTED_EDGE('',*,*,#8372,.F.);
#10875=ORIENTED_EDGE('',*,*,#8369,.F.);
#10876=ORIENTED_EDGE('',*,*,#8373,.F.);
#10877=ORIENTED_EDGE('',*,*,#8374,.T.);
#10878=ORIENTED_EDGE('',*,*,#8375,.F.);
#10879=ORIENTED_EDGE('',*,*,#8374,.F.);
#10880=ORIENTED_EDGE('',*,*,#8376,.F.);
#10881=ORIENTED_EDGE('',*,*,#8377,.T.);
#10882=ORIENTED_EDGE('',*,*,#8378,.F.);
#10883=ORIENTED_EDGE('',*,*,#8379,.F.);
#10884=ORIENTED_EDGE('',*,*,#8380,.F.);
#10885=ORIENTED_EDGE('',*,*,#8381,.F.);
#10886=ORIENTED_EDGE('',*,*,#8382,.F.);
#10887=ORIENTED_EDGE('',*,*,#8383,.T.);
#10888=ORIENTED_EDGE('',*,*,#8382,.T.);
#10889=ORIENTED_EDGE('',*,*,#8384,.F.);
#10890=ORIENTED_EDGE('',*,*,#8385,.T.);
#10891=ORIENTED_EDGE('',*,*,#8386,.T.);
#10892=ORIENTED_EDGE('',*,*,#8380,.T.);
#10893=ORIENTED_EDGE('',*,*,#8387,.T.);
#10894=ORIENTED_EDGE('',*,*,#8388,.T.);
#10895=ORIENTED_EDGE('',*,*,#8389,.F.);
#10896=ORIENTED_EDGE('',*,*,#8378,.T.);
#10897=ORIENTED_EDGE('',*,*,#8390,.T.);
#10898=ORIENTED_EDGE('',*,*,#8391,.T.);
#10899=ORIENTED_EDGE('',*,*,#8392,.F.);
#10900=ORIENTED_EDGE('',*,*,#8393,.F.);
#10901=ORIENTED_EDGE('',*,*,#8394,.T.);
#10902=ORIENTED_EDGE('',*,*,#8395,.F.);
#10903=ORIENTED_EDGE('',*,*,#8394,.F.);
#10904=ORIENTED_EDGE('',*,*,#8385,.F.);
#10905=ORIENTED_EDGE('',*,*,#8396,.F.);
#10906=ORIENTED_EDGE('',*,*,#8391,.F.);
#10907=ORIENTED_EDGE('',*,*,#8397,.T.);
#10908=ORIENTED_EDGE('',*,*,#8398,.F.);
#10909=ORIENTED_EDGE('',*,*,#8399,.F.);
#10910=ORIENTED_EDGE('',*,*,#8387,.F.);
#10911=ORIENTED_EDGE('',*,*,#8383,.F.);
#10912=ORIENTED_EDGE('',*,*,#8386,.F.);
#10913=ORIENTED_EDGE('',*,*,#8397,.F.);
#10914=ORIENTED_EDGE('',*,*,#8390,.F.);
#10915=ORIENTED_EDGE('',*,*,#8377,.F.);
#10916=ORIENTED_EDGE('',*,*,#8373,.T.);
#10917=ORIENTED_EDGE('',*,*,#8393,.T.);
#10918=ORIENTED_EDGE('',*,*,#8400,.T.);
#10919=ORIENTED_EDGE('',*,*,#8376,.T.);
#10920=ORIENTED_EDGE('',*,*,#8401,.F.);
#10921=ORIENTED_EDGE('',*,*,#8402,.T.);
#10922=ORIENTED_EDGE('',*,*,#8398,.T.);
#10923=ORIENTED_EDGE('',*,*,#8400,.F.);
#10924=ORIENTED_EDGE('',*,*,#8403,.T.);
#10925=ORIENTED_EDGE('',*,*,#8404,.F.);
#10926=ORIENTED_EDGE('',*,*,#8403,.F.);
#10927=ORIENTED_EDGE('',*,*,#8388,.F.);
#10928=ORIENTED_EDGE('',*,*,#8399,.T.);
#10929=ORIENTED_EDGE('',*,*,#8402,.F.);
#10930=ORIENTED_EDGE('',*,*,#8405,.F.);
#10931=ORIENTED_EDGE('',*,*,#8389,.T.);
#10932=ORIENTED_EDGE('',*,*,#8405,.T.);
#10933=ORIENTED_EDGE('',*,*,#8401,.T.);
#10934=ORIENTED_EDGE('',*,*,#8379,.T.);
#10935=ORIENTED_EDGE('',*,*,#8392,.T.);
#10936=ORIENTED_EDGE('',*,*,#8396,.T.);
#10937=ORIENTED_EDGE('',*,*,#8384,.T.);
#10938=ORIENTED_EDGE('',*,*,#8381,.T.);
#10939=ORIENTED_EDGE('',*,*,#8375,.T.);
#10940=ORIENTED_EDGE('',*,*,#8395,.T.);
#10941=ORIENTED_EDGE('',*,*,#8404,.T.);
#10942=ORIENTED_EDGE('',*,*,#8406,.F.);
#10943=ORIENTED_EDGE('',*,*,#8407,.T.);
#10944=ORIENTED_EDGE('',*,*,#8408,.T.);
#10945=ORIENTED_EDGE('',*,*,#8407,.F.);
#10946=ORIENTED_EDGE('',*,*,#8409,.F.);
#10947=ORIENTED_EDGE('',*,*,#8410,.T.);
#10948=ORIENTED_EDGE('',*,*,#8411,.T.);
#10949=ORIENTED_EDGE('',*,*,#8410,.F.);
#10950=ORIENTED_EDGE('',*,*,#8409,.T.);
#10951=ORIENTED_EDGE('',*,*,#8406,.T.);
#10952=ORIENTED_EDGE('',*,*,#8411,.F.);
#10953=ORIENTED_EDGE('',*,*,#8408,.F.);
#10954=ORIENTED_EDGE('',*,*,#8412,.F.);
#10955=ORIENTED_EDGE('',*,*,#8413,.T.);
#10956=ORIENTED_EDGE('',*,*,#8414,.T.);
#10957=ORIENTED_EDGE('',*,*,#8413,.F.);
#10958=ORIENTED_EDGE('',*,*,#8415,.F.);
#10959=ORIENTED_EDGE('',*,*,#8416,.T.);
#10960=ORIENTED_EDGE('',*,*,#8417,.T.);
#10961=ORIENTED_EDGE('',*,*,#8416,.F.);
#10962=ORIENTED_EDGE('',*,*,#8415,.T.);
#10963=ORIENTED_EDGE('',*,*,#8412,.T.);
#10964=ORIENTED_EDGE('',*,*,#8417,.F.);
#10965=ORIENTED_EDGE('',*,*,#8414,.F.);
#10966=ORIENTED_EDGE('',*,*,#8418,.F.);
#10967=ORIENTED_EDGE('',*,*,#8419,.T.);
#10968=ORIENTED_EDGE('',*,*,#8420,.T.);
#10969=ORIENTED_EDGE('',*,*,#8419,.F.);
#10970=ORIENTED_EDGE('',*,*,#8421,.F.);
#10971=ORIENTED_EDGE('',*,*,#8422,.T.);
#10972=ORIENTED_EDGE('',*,*,#8423,.T.);
#10973=ORIENTED_EDGE('',*,*,#8422,.F.);
#10974=ORIENTED_EDGE('',*,*,#8421,.T.);
#10975=ORIENTED_EDGE('',*,*,#8418,.T.);
#10976=ORIENTED_EDGE('',*,*,#8423,.F.);
#10977=ORIENTED_EDGE('',*,*,#8420,.F.);
#10978=ORIENTED_EDGE('',*,*,#8424,.F.);
#10979=ORIENTED_EDGE('',*,*,#8425,.T.);
#10980=ORIENTED_EDGE('',*,*,#8426,.F.);
#10981=ORIENTED_EDGE('',*,*,#8425,.F.);
#10982=ORIENTED_EDGE('',*,*,#8424,.T.);
#10983=ORIENTED_EDGE('',*,*,#8427,.F.);
#10984=ORIENTED_EDGE('',*,*,#8428,.T.);
#10985=ORIENTED_EDGE('',*,*,#8429,.T.);
#10986=ORIENTED_EDGE('',*,*,#8428,.F.);
#10987=ORIENTED_EDGE('',*,*,#8429,.F.);
#10988=ORIENTED_EDGE('',*,*,#8430,.F.);
#10989=ORIENTED_EDGE('',*,*,#8431,.T.);
#10990=ORIENTED_EDGE('',*,*,#8432,.T.);
#10991=ORIENTED_EDGE('',*,*,#8431,.F.);
#10992=ORIENTED_EDGE('',*,*,#8430,.T.);
#10993=ORIENTED_EDGE('',*,*,#8426,.T.);
#10994=ORIENTED_EDGE('',*,*,#8432,.F.);
#10995=ORIENTED_EDGE('',*,*,#8427,.T.);
#10996=ORIENTED_EDGE('',*,*,#8433,.F.);
#10997=ORIENTED_EDGE('',*,*,#8434,.T.);
#10998=ORIENTED_EDGE('',*,*,#8435,.T.);
#10999=ORIENTED_EDGE('',*,*,#8434,.F.);
#11000=ORIENTED_EDGE('',*,*,#8436,.F.);
#11001=ORIENTED_EDGE('',*,*,#8437,.T.);
#11002=ORIENTED_EDGE('',*,*,#8438,.T.);
#11003=ORIENTED_EDGE('',*,*,#8437,.F.);
#11004=ORIENTED_EDGE('',*,*,#8436,.T.);
#11005=ORIENTED_EDGE('',*,*,#8433,.T.);
#11006=ORIENTED_EDGE('',*,*,#8438,.F.);
#11007=ORIENTED_EDGE('',*,*,#8435,.F.);
#11008=ORIENTED_EDGE('',*,*,#8439,.F.);
#11009=ORIENTED_EDGE('',*,*,#8440,.T.);
#11010=ORIENTED_EDGE('',*,*,#8441,.T.);
#11011=ORIENTED_EDGE('',*,*,#8440,.F.);
#11012=ORIENTED_EDGE('',*,*,#8442,.F.);
#11013=ORIENTED_EDGE('',*,*,#8443,.T.);
#11014=ORIENTED_EDGE('',*,*,#8444,.T.);
#11015=ORIENTED_EDGE('',*,*,#8443,.F.);
#11016=ORIENTED_EDGE('',*,*,#8442,.T.);
#11017=ORIENTED_EDGE('',*,*,#8439,.T.);
#11018=ORIENTED_EDGE('',*,*,#8444,.F.);
#11019=ORIENTED_EDGE('',*,*,#8441,.F.);
#11020=ORIENTED_EDGE('',*,*,#8445,.F.);
#11021=ORIENTED_EDGE('',*,*,#8446,.T.);
#11022=ORIENTED_EDGE('',*,*,#8447,.T.);
#11023=ORIENTED_EDGE('',*,*,#8446,.F.);
#11024=ORIENTED_EDGE('',*,*,#8448,.F.);
#11025=ORIENTED_EDGE('',*,*,#8449,.T.);
#11026=ORIENTED_EDGE('',*,*,#8450,.T.);
#11027=ORIENTED_EDGE('',*,*,#8449,.F.);
#11028=ORIENTED_EDGE('',*,*,#8448,.T.);
#11029=ORIENTED_EDGE('',*,*,#8445,.T.);
#11030=ORIENTED_EDGE('',*,*,#8450,.F.);
#11031=ORIENTED_EDGE('',*,*,#8447,.F.);
#11032=ORIENTED_EDGE('',*,*,#8451,.F.);
#11033=ORIENTED_EDGE('',*,*,#8452,.T.);
#11034=ORIENTED_EDGE('',*,*,#8453,.T.);
#11035=ORIENTED_EDGE('',*,*,#8452,.F.);
#11036=ORIENTED_EDGE('',*,*,#8454,.F.);
#11037=ORIENTED_EDGE('',*,*,#8455,.T.);
#11038=ORIENTED_EDGE('',*,*,#8456,.T.);
#11039=ORIENTED_EDGE('',*,*,#8455,.F.);
#11040=ORIENTED_EDGE('',*,*,#8454,.T.);
#11041=ORIENTED_EDGE('',*,*,#8451,.T.);
#11042=ORIENTED_EDGE('',*,*,#8456,.F.);
#11043=ORIENTED_EDGE('',*,*,#8453,.F.);
#11044=ORIENTED_EDGE('',*,*,#8457,.F.);
#11045=ORIENTED_EDGE('',*,*,#8458,.T.);
#11046=ORIENTED_EDGE('',*,*,#8459,.T.);
#11047=ORIENTED_EDGE('',*,*,#8458,.F.);
#11048=ORIENTED_EDGE('',*,*,#8460,.F.);
#11049=ORIENTED_EDGE('',*,*,#8461,.T.);
#11050=ORIENTED_EDGE('',*,*,#8462,.T.);
#11051=ORIENTED_EDGE('',*,*,#8461,.F.);
#11052=ORIENTED_EDGE('',*,*,#8460,.T.);
#11053=ORIENTED_EDGE('',*,*,#8457,.T.);
#11054=ORIENTED_EDGE('',*,*,#8462,.F.);
#11055=ORIENTED_EDGE('',*,*,#8459,.F.);
#11056=ORIENTED_EDGE('',*,*,#8463,.F.);
#11057=ORIENTED_EDGE('',*,*,#8464,.T.);
#11058=ORIENTED_EDGE('',*,*,#8465,.T.);
#11059=ORIENTED_EDGE('',*,*,#8464,.F.);
#11060=ORIENTED_EDGE('',*,*,#8466,.F.);
#11061=ORIENTED_EDGE('',*,*,#8467,.T.);
#11062=ORIENTED_EDGE('',*,*,#8468,.T.);
#11063=ORIENTED_EDGE('',*,*,#8467,.F.);
#11064=ORIENTED_EDGE('',*,*,#8466,.T.);
#11065=ORIENTED_EDGE('',*,*,#8463,.T.);
#11066=ORIENTED_EDGE('',*,*,#8468,.F.);
#11067=ORIENTED_EDGE('',*,*,#8465,.F.);
#11068=ORIENTED_EDGE('',*,*,#8469,.F.);
#11069=ORIENTED_EDGE('',*,*,#8470,.T.);
#11070=ORIENTED_EDGE('',*,*,#8471,.T.);
#11071=ORIENTED_EDGE('',*,*,#8470,.F.);
#11072=ORIENTED_EDGE('',*,*,#8472,.F.);
#11073=ORIENTED_EDGE('',*,*,#8473,.T.);
#11074=ORIENTED_EDGE('',*,*,#8474,.T.);
#11075=ORIENTED_EDGE('',*,*,#8473,.F.);
#11076=ORIENTED_EDGE('',*,*,#8472,.T.);
#11077=ORIENTED_EDGE('',*,*,#8469,.T.);
#11078=ORIENTED_EDGE('',*,*,#8474,.F.);
#11079=ORIENTED_EDGE('',*,*,#8471,.F.);
#11080=ORIENTED_EDGE('',*,*,#8475,.F.);
#11081=ORIENTED_EDGE('',*,*,#8476,.F.);
#11082=ORIENTED_EDGE('',*,*,#8477,.T.);
#11083=ORIENTED_EDGE('',*,*,#8475,.T.);
#11084=ORIENTED_EDGE('',*,*,#8477,.F.);
#11085=ORIENTED_EDGE('',*,*,#8478,.F.);
#11086=ORIENTED_EDGE('',*,*,#8479,.T.);
#11087=ORIENTED_EDGE('',*,*,#8476,.T.);
#11088=ORIENTED_EDGE('',*,*,#8479,.F.);
#11089=ORIENTED_EDGE('',*,*,#8480,.F.);
#11090=ORIENTED_EDGE('',*,*,#8481,.T.);
#11091=ORIENTED_EDGE('',*,*,#8478,.T.);
#11092=ORIENTED_EDGE('',*,*,#8481,.F.);
#11093=ORIENTED_EDGE('',*,*,#8480,.T.);
#11094=ORIENTED_EDGE('',*,*,#8482,.F.);
#11095=ORIENTED_EDGE('',*,*,#8483,.F.);
#11096=ORIENTED_EDGE('',*,*,#8484,.T.);
#11097=ORIENTED_EDGE('',*,*,#8482,.T.);
#11098=ORIENTED_EDGE('',*,*,#8484,.F.);
#11099=ORIENTED_EDGE('',*,*,#8485,.F.);
#11100=ORIENTED_EDGE('',*,*,#8486,.T.);
#11101=ORIENTED_EDGE('',*,*,#8483,.T.);
#11102=ORIENTED_EDGE('',*,*,#8486,.F.);
#11103=ORIENTED_EDGE('',*,*,#8487,.F.);
#11104=ORIENTED_EDGE('',*,*,#8488,.T.);
#11105=ORIENTED_EDGE('',*,*,#8485,.T.);
#11106=ORIENTED_EDGE('',*,*,#8488,.F.);
#11107=ORIENTED_EDGE('',*,*,#8487,.T.);
#11108=ORIENTED_EDGE('',*,*,#8489,.T.);
#11109=ORIENTED_EDGE('',*,*,#8490,.T.);
#11110=ORIENTED_EDGE('',*,*,#8491,.T.);
#11111=ORIENTED_EDGE('',*,*,#8492,.F.);
#11112=ORIENTED_EDGE('',*,*,#8493,.T.);
#11113=ORIENTED_EDGE('',*,*,#8494,.T.);
#11114=ORIENTED_EDGE('',*,*,#8495,.T.);
#11115=ORIENTED_EDGE('',*,*,#8490,.F.);
#11116=ORIENTED_EDGE('',*,*,#8496,.T.);
#11117=ORIENTED_EDGE('',*,*,#8497,.T.);
#11118=ORIENTED_EDGE('',*,*,#8498,.T.);
#11119=ORIENTED_EDGE('',*,*,#8494,.F.);
#11120=ORIENTED_EDGE('',*,*,#8499,.T.);
#11121=ORIENTED_EDGE('',*,*,#8500,.T.);
#11122=ORIENTED_EDGE('',*,*,#8501,.T.);
#11123=ORIENTED_EDGE('',*,*,#8497,.F.);
#11124=ORIENTED_EDGE('',*,*,#8502,.T.);
#11125=ORIENTED_EDGE('',*,*,#8503,.T.);
#11126=ORIENTED_EDGE('',*,*,#8504,.T.);
#11127=ORIENTED_EDGE('',*,*,#8500,.F.);
#11128=ORIENTED_EDGE('',*,*,#8505,.T.);
#11129=ORIENTED_EDGE('',*,*,#8492,.T.);
#11130=ORIENTED_EDGE('',*,*,#8506,.T.);
#11131=ORIENTED_EDGE('',*,*,#8503,.F.);
#11132=ORIENTED_EDGE('',*,*,#8505,.F.);
#11133=ORIENTED_EDGE('',*,*,#8502,.F.);
#11134=ORIENTED_EDGE('',*,*,#8499,.F.);
#11135=ORIENTED_EDGE('',*,*,#8496,.F.);
#11136=ORIENTED_EDGE('',*,*,#8493,.F.);
#11137=ORIENTED_EDGE('',*,*,#8489,.F.);
#11138=ORIENTED_EDGE('',*,*,#8506,.F.);
#11139=ORIENTED_EDGE('',*,*,#8491,.F.);
#11140=ORIENTED_EDGE('',*,*,#8495,.F.);
#11141=ORIENTED_EDGE('',*,*,#8498,.F.);
#11142=ORIENTED_EDGE('',*,*,#8501,.F.);
#11143=ORIENTED_EDGE('',*,*,#8504,.F.);
#11144=ORIENTED_EDGE('',*,*,#8507,.F.);
#11145=ORIENTED_EDGE('',*,*,#8508,.T.);
#11146=ORIENTED_EDGE('',*,*,#8509,.F.);
#11147=ORIENTED_EDGE('',*,*,#8508,.F.);
#11148=ORIENTED_EDGE('',*,*,#8510,.F.);
#11149=ORIENTED_EDGE('',*,*,#8511,.T.);
#11150=ORIENTED_EDGE('',*,*,#8512,.F.);
#11151=ORIENTED_EDGE('',*,*,#8511,.F.);
#11152=ORIENTED_EDGE('',*,*,#8513,.F.);
#11153=ORIENTED_EDGE('',*,*,#8514,.T.);
#11154=ORIENTED_EDGE('',*,*,#8515,.F.);
#11155=ORIENTED_EDGE('',*,*,#8514,.F.);
#11156=ORIENTED_EDGE('',*,*,#8516,.F.);
#11157=ORIENTED_EDGE('',*,*,#8517,.T.);
#11158=ORIENTED_EDGE('',*,*,#8518,.F.);
#11159=ORIENTED_EDGE('',*,*,#8517,.F.);
#11160=ORIENTED_EDGE('',*,*,#8519,.F.);
#11161=ORIENTED_EDGE('',*,*,#8520,.T.);
#11162=ORIENTED_EDGE('',*,*,#8521,.F.);
#11163=ORIENTED_EDGE('',*,*,#8520,.F.);
#11164=ORIENTED_EDGE('',*,*,#8522,.F.);
#11165=ORIENTED_EDGE('',*,*,#8523,.F.);
#11166=ORIENTED_EDGE('',*,*,#8524,.F.);
#11167=ORIENTED_EDGE('',*,*,#8525,.T.);
#11168=ORIENTED_EDGE('',*,*,#8526,.F.);
#11169=ORIENTED_EDGE('',*,*,#8527,.T.);
#11170=ORIENTED_EDGE('',*,*,#8528,.F.);
#11171=ORIENTED_EDGE('',*,*,#8529,.F.);
#11172=ORIENTED_EDGE('',*,*,#8528,.T.);
#11173=ORIENTED_EDGE('',*,*,#8530,.T.);
#11174=ORIENTED_EDGE('',*,*,#8531,.T.);
#11175=ORIENTED_EDGE('',*,*,#8532,.F.);
#11176=ORIENTED_EDGE('',*,*,#8532,.T.);
#11177=ORIENTED_EDGE('',*,*,#8533,.T.);
#11178=ORIENTED_EDGE('',*,*,#8534,.T.);
#11179=ORIENTED_EDGE('',*,*,#8523,.T.);
#11180=ORIENTED_EDGE('',*,*,#8535,.T.);
#11181=ORIENTED_EDGE('',*,*,#8536,.T.);
#11182=ORIENTED_EDGE('',*,*,#8537,.T.);
#11183=ORIENTED_EDGE('',*,*,#8529,.T.);
#11184=ORIENTED_EDGE('',*,*,#8538,.T.);
#11185=ORIENTED_EDGE('',*,*,#8539,.T.);
#11186=ORIENTED_EDGE('',*,*,#8521,.T.);
#11187=ORIENTED_EDGE('',*,*,#8518,.T.);
#11188=ORIENTED_EDGE('',*,*,#8515,.T.);
#11189=ORIENTED_EDGE('',*,*,#8512,.T.);
#11190=ORIENTED_EDGE('',*,*,#8509,.T.);
#11191=ORIENTED_EDGE('',*,*,#8524,.T.);
#11192=ORIENTED_EDGE('',*,*,#8534,.F.);
#11193=ORIENTED_EDGE('',*,*,#8540,.T.);
#11194=ORIENTED_EDGE('',*,*,#8541,.T.);
#11195=ORIENTED_EDGE('',*,*,#8542,.F.);
#11196=ORIENTED_EDGE('',*,*,#8543,.T.);
#11197=ORIENTED_EDGE('',*,*,#8538,.F.);
#11198=ORIENTED_EDGE('',*,*,#8543,.F.);
#11199=ORIENTED_EDGE('',*,*,#8544,.F.);
#11200=ORIENTED_EDGE('',*,*,#8545,.T.);
#11201=ORIENTED_EDGE('',*,*,#8546,.F.);
#11202=ORIENTED_EDGE('',*,*,#8536,.F.);
#11203=ORIENTED_EDGE('',*,*,#8522,.T.);
#11204=ORIENTED_EDGE('',*,*,#8547,.T.);
#11205=ORIENTED_EDGE('',*,*,#8544,.T.);
#11206=ORIENTED_EDGE('',*,*,#8535,.F.);
#11207=ORIENTED_EDGE('',*,*,#8548,.F.);
#11208=ORIENTED_EDGE('',*,*,#8549,.T.);
#11209=ORIENTED_EDGE('',*,*,#8539,.F.);
#11210=ORIENTED_EDGE('',*,*,#8549,.F.);
#11211=ORIENTED_EDGE('',*,*,#8531,.F.);
#11212=ORIENTED_EDGE('',*,*,#8550,.T.);
#11213=ORIENTED_EDGE('',*,*,#8540,.F.);
#11214=ORIENTED_EDGE('',*,*,#8533,.F.);
#11215=ORIENTED_EDGE('',*,*,#8526,.T.);
#11216=ORIENTED_EDGE('',*,*,#8537,.F.);
#11217=ORIENTED_EDGE('',*,*,#8546,.T.);
#11218=ORIENTED_EDGE('',*,*,#8551,.T.);
#11219=ORIENTED_EDGE('',*,*,#8551,.F.);
#11220=ORIENTED_EDGE('',*,*,#8545,.F.);
#11221=ORIENTED_EDGE('',*,*,#8547,.F.);
#11222=ORIENTED_EDGE('',*,*,#8525,.F.);
#11223=ORIENTED_EDGE('',*,*,#8541,.F.);
#11224=ORIENTED_EDGE('',*,*,#8550,.F.);
#11225=ORIENTED_EDGE('',*,*,#8530,.F.);
#11226=ORIENTED_EDGE('',*,*,#8527,.F.);
#11227=ORIENTED_EDGE('',*,*,#8542,.T.);
#11228=ORIENTED_EDGE('',*,*,#8548,.T.);
#11229=ORIENTED_EDGE('',*,*,#8519,.T.);
#11230=ORIENTED_EDGE('',*,*,#8516,.T.);
#11231=ORIENTED_EDGE('',*,*,#8513,.T.);
#11232=ORIENTED_EDGE('',*,*,#8510,.T.);
#11233=ORIENTED_EDGE('',*,*,#8507,.T.);
#11234=ORIENTED_EDGE('',*,*,#8552,.F.);
#11235=ORIENTED_EDGE('',*,*,#8553,.T.);
#11236=ORIENTED_EDGE('',*,*,#8554,.T.);
#11237=ORIENTED_EDGE('',*,*,#8553,.F.);
#11238=ORIENTED_EDGE('',*,*,#8555,.F.);
#11239=ORIENTED_EDGE('',*,*,#8556,.T.);
#11240=ORIENTED_EDGE('',*,*,#8557,.T.);
#11241=ORIENTED_EDGE('',*,*,#8556,.F.);
#11242=ORIENTED_EDGE('',*,*,#8555,.T.);
#11243=ORIENTED_EDGE('',*,*,#8552,.T.);
#11244=ORIENTED_EDGE('',*,*,#8557,.F.);
#11245=ORIENTED_EDGE('',*,*,#8554,.F.);
#11246=ORIENTED_EDGE('',*,*,#8558,.F.);
#11247=ORIENTED_EDGE('',*,*,#8559,.T.);
#11248=ORIENTED_EDGE('',*,*,#8560,.T.);
#11249=ORIENTED_EDGE('',*,*,#8559,.F.);
#11250=ORIENTED_EDGE('',*,*,#8561,.F.);
#11251=ORIENTED_EDGE('',*,*,#8562,.T.);
#11252=ORIENTED_EDGE('',*,*,#8563,.T.);
#11253=ORIENTED_EDGE('',*,*,#8562,.F.);
#11254=ORIENTED_EDGE('',*,*,#8561,.T.);
#11255=ORIENTED_EDGE('',*,*,#8558,.T.);
#11256=ORIENTED_EDGE('',*,*,#8563,.F.);
#11257=ORIENTED_EDGE('',*,*,#8560,.F.);
#11258=ORIENTED_EDGE('',*,*,#8564,.F.);
#11259=ORIENTED_EDGE('',*,*,#8565,.T.);
#11260=ORIENTED_EDGE('',*,*,#8566,.F.);
#11261=ORIENTED_EDGE('',*,*,#8565,.F.);
#11262=ORIENTED_EDGE('',*,*,#8567,.F.);
#11263=ORIENTED_EDGE('',*,*,#8568,.T.);
#11264=ORIENTED_EDGE('',*,*,#8569,.F.);
#11265=ORIENTED_EDGE('',*,*,#8568,.F.);
#11266=ORIENTED_EDGE('',*,*,#8570,.F.);
#11267=ORIENTED_EDGE('',*,*,#8571,.T.);
#11268=ORIENTED_EDGE('',*,*,#8572,.F.);
#11269=ORIENTED_EDGE('',*,*,#8571,.F.);
#11270=ORIENTED_EDGE('',*,*,#8573,.F.);
#11271=ORIENTED_EDGE('',*,*,#8574,.T.);
#11272=ORIENTED_EDGE('',*,*,#8575,.F.);
#11273=ORIENTED_EDGE('',*,*,#8574,.F.);
#11274=ORIENTED_EDGE('',*,*,#8576,.F.);
#11275=ORIENTED_EDGE('',*,*,#8577,.T.);
#11276=ORIENTED_EDGE('',*,*,#8578,.T.);
#11277=ORIENTED_EDGE('',*,*,#8577,.F.);
#11278=ORIENTED_EDGE('',*,*,#8579,.F.);
#11279=ORIENTED_EDGE('',*,*,#8580,.T.);
#11280=ORIENTED_EDGE('',*,*,#8581,.T.);
#11281=ORIENTED_EDGE('',*,*,#8580,.F.);
#11282=ORIENTED_EDGE('',*,*,#8579,.T.);
#11283=ORIENTED_EDGE('',*,*,#8576,.T.);
#11284=ORIENTED_EDGE('',*,*,#8575,.T.);
#11285=ORIENTED_EDGE('',*,*,#8572,.T.);
#11286=ORIENTED_EDGE('',*,*,#8569,.T.);
#11287=ORIENTED_EDGE('',*,*,#8566,.T.);
#11288=ORIENTED_EDGE('',*,*,#8581,.F.);
#11289=ORIENTED_EDGE('',*,*,#8578,.F.);
#11290=ORIENTED_EDGE('',*,*,#8573,.T.);
#11291=ORIENTED_EDGE('',*,*,#8570,.T.);
#11292=ORIENTED_EDGE('',*,*,#8567,.T.);
#11293=ORIENTED_EDGE('',*,*,#8564,.T.);
#11294=ORIENTED_EDGE('',*,*,#8582,.T.);
#11295=ORIENTED_EDGE('',*,*,#8583,.F.);
#11296=ORIENTED_EDGE('',*,*,#8582,.F.);
#11297=ORIENTED_EDGE('',*,*,#8584,.T.);
#11298=ORIENTED_EDGE('',*,*,#8585,.T.);
#11299=ORIENTED_EDGE('',*,*,#8584,.F.);
#11300=ORIENTED_EDGE('',*,*,#8585,.F.);
#11301=ORIENTED_EDGE('',*,*,#8586,.F.);
#11302=ORIENTED_EDGE('',*,*,#8587,.T.);
#11303=ORIENTED_EDGE('',*,*,#8583,.T.);
#11304=ORIENTED_EDGE('',*,*,#8587,.F.);
#11305=ORIENTED_EDGE('',*,*,#8586,.T.);
#11306=ORIENTED_EDGE('',*,*,#8588,.T.);
#11307=ORIENTED_EDGE('',*,*,#8589,.F.);
#11308=ORIENTED_EDGE('',*,*,#8588,.F.);
#11309=ORIENTED_EDGE('',*,*,#8590,.T.);
#11310=ORIENTED_EDGE('',*,*,#8591,.T.);
#11311=ORIENTED_EDGE('',*,*,#8590,.F.);
#11312=ORIENTED_EDGE('',*,*,#8591,.F.);
#11313=ORIENTED_EDGE('',*,*,#8592,.F.);
#11314=ORIENTED_EDGE('',*,*,#8593,.T.);
#11315=ORIENTED_EDGE('',*,*,#8589,.T.);
#11316=ORIENTED_EDGE('',*,*,#8593,.F.);
#11317=ORIENTED_EDGE('',*,*,#8592,.T.);
#11318=ORIENTED_EDGE('',*,*,#8594,.T.);
#11319=ORIENTED_EDGE('',*,*,#8595,.F.);
#11320=ORIENTED_EDGE('',*,*,#8594,.F.);
#11321=ORIENTED_EDGE('',*,*,#8596,.T.);
#11322=ORIENTED_EDGE('',*,*,#8597,.T.);
#11323=ORIENTED_EDGE('',*,*,#8596,.F.);
#11324=ORIENTED_EDGE('',*,*,#8597,.F.);
#11325=ORIENTED_EDGE('',*,*,#8598,.F.);
#11326=ORIENTED_EDGE('',*,*,#8599,.T.);
#11327=ORIENTED_EDGE('',*,*,#8595,.T.);
#11328=ORIENTED_EDGE('',*,*,#8599,.F.);
#11329=ORIENTED_EDGE('',*,*,#8598,.T.);
#11330=ORIENTED_EDGE('',*,*,#8600,.T.);
#11331=ORIENTED_EDGE('',*,*,#8601,.F.);
#11332=ORIENTED_EDGE('',*,*,#8600,.F.);
#11333=ORIENTED_EDGE('',*,*,#8602,.T.);
#11334=ORIENTED_EDGE('',*,*,#8603,.T.);
#11335=ORIENTED_EDGE('',*,*,#8602,.F.);
#11336=ORIENTED_EDGE('',*,*,#8603,.F.);
#11337=ORIENTED_EDGE('',*,*,#8604,.F.);
#11338=ORIENTED_EDGE('',*,*,#8605,.T.);
#11339=ORIENTED_EDGE('',*,*,#8601,.T.);
#11340=ORIENTED_EDGE('',*,*,#8605,.F.);
#11341=ORIENTED_EDGE('',*,*,#8604,.T.);
#11342=ORIENTED_EDGE('',*,*,#8606,.F.);
#11343=ORIENTED_EDGE('',*,*,#8607,.T.);
#11344=ORIENTED_EDGE('',*,*,#8608,.F.);
#11345=ORIENTED_EDGE('',*,*,#8607,.F.);
#11346=ORIENTED_EDGE('',*,*,#8609,.F.);
#11347=ORIENTED_EDGE('',*,*,#8610,.T.);
#11348=ORIENTED_EDGE('',*,*,#8611,.F.);
#11349=ORIENTED_EDGE('',*,*,#8610,.F.);
#11350=ORIENTED_EDGE('',*,*,#8612,.F.);
#11351=ORIENTED_EDGE('',*,*,#8613,.T.);
#11352=ORIENTED_EDGE('',*,*,#8614,.F.);
#11353=ORIENTED_EDGE('',*,*,#8613,.F.);
#11354=ORIENTED_EDGE('',*,*,#8615,.F.);
#11355=ORIENTED_EDGE('',*,*,#8616,.T.);
#11356=ORIENTED_EDGE('',*,*,#8617,.F.);
#11357=ORIENTED_EDGE('',*,*,#8616,.F.);
#11358=ORIENTED_EDGE('',*,*,#8618,.F.);
#11359=ORIENTED_EDGE('',*,*,#8619,.T.);
#11360=ORIENTED_EDGE('',*,*,#8620,.T.);
#11361=ORIENTED_EDGE('',*,*,#8619,.F.);
#11362=ORIENTED_EDGE('',*,*,#8621,.F.);
#11363=ORIENTED_EDGE('',*,*,#8622,.T.);
#11364=ORIENTED_EDGE('',*,*,#8623,.T.);
#11365=ORIENTED_EDGE('',*,*,#8622,.F.);
#11366=ORIENTED_EDGE('',*,*,#8621,.T.);
#11367=ORIENTED_EDGE('',*,*,#8618,.T.);
#11368=ORIENTED_EDGE('',*,*,#8617,.T.);
#11369=ORIENTED_EDGE('',*,*,#8614,.T.);
#11370=ORIENTED_EDGE('',*,*,#8611,.T.);
#11371=ORIENTED_EDGE('',*,*,#8608,.T.);
#11372=ORIENTED_EDGE('',*,*,#8623,.F.);
#11373=ORIENTED_EDGE('',*,*,#8620,.F.);
#11374=ORIENTED_EDGE('',*,*,#8615,.T.);
#11375=ORIENTED_EDGE('',*,*,#8612,.T.);
#11376=ORIENTED_EDGE('',*,*,#8609,.T.);
#11377=ORIENTED_EDGE('',*,*,#8606,.T.);
#11378=ORIENTED_EDGE('',*,*,#8624,.F.);
#11379=ORIENTED_EDGE('',*,*,#8625,.T.);
#11380=ORIENTED_EDGE('',*,*,#8626,.F.);
#11381=ORIENTED_EDGE('',*,*,#8627,.T.);
#11382=ORIENTED_EDGE('',*,*,#8624,.T.);
#11383=ORIENTED_EDGE('',*,*,#8627,.F.);
#11384=ORIENTED_EDGE('',*,*,#8626,.T.);
#11385=ORIENTED_EDGE('',*,*,#8625,.F.);
#11386=ORIENTED_EDGE('',*,*,#8628,.T.);
#11387=ORIENTED_EDGE('',*,*,#8629,.T.);
#11388=ORIENTED_EDGE('',*,*,#8628,.F.);
#11389=ORIENTED_EDGE('',*,*,#8629,.F.);
#11390=ORIENTED_EDGE('',*,*,#8630,.F.);
#11391=ORIENTED_EDGE('',*,*,#8631,.T.);
#11392=ORIENTED_EDGE('',*,*,#8632,.F.);
#11393=ORIENTED_EDGE('',*,*,#8633,.T.);
#11394=ORIENTED_EDGE('',*,*,#8630,.T.);
#11395=ORIENTED_EDGE('',*,*,#8633,.F.);
#11396=ORIENTED_EDGE('',*,*,#8632,.T.);
#11397=ORIENTED_EDGE('',*,*,#8631,.F.);
#11398=ORIENTED_EDGE('',*,*,#8634,.T.);
#11399=ORIENTED_EDGE('',*,*,#8635,.T.);
#11400=ORIENTED_EDGE('',*,*,#8634,.F.);
#11401=ORIENTED_EDGE('',*,*,#8635,.F.);
#11402=ORIENTED_EDGE('',*,*,#8636,.F.);
#11403=ORIENTED_EDGE('',*,*,#8637,.T.);
#11404=ORIENTED_EDGE('',*,*,#8638,.F.);
#11405=ORIENTED_EDGE('',*,*,#8639,.T.);
#11406=ORIENTED_EDGE('',*,*,#8636,.T.);
#11407=ORIENTED_EDGE('',*,*,#8639,.F.);
#11408=ORIENTED_EDGE('',*,*,#8638,.T.);
#11409=ORIENTED_EDGE('',*,*,#8637,.F.);
#11410=ORIENTED_EDGE('',*,*,#8640,.T.);
#11411=ORIENTED_EDGE('',*,*,#8641,.T.);
#11412=ORIENTED_EDGE('',*,*,#8640,.F.);
#11413=ORIENTED_EDGE('',*,*,#8641,.F.);
#11414=ORIENTED_EDGE('',*,*,#8642,.F.);
#11415=ORIENTED_EDGE('',*,*,#8643,.T.);
#11416=ORIENTED_EDGE('',*,*,#8644,.F.);
#11417=ORIENTED_EDGE('',*,*,#8645,.T.);
#11418=ORIENTED_EDGE('',*,*,#8642,.T.);
#11419=ORIENTED_EDGE('',*,*,#8645,.F.);
#11420=ORIENTED_EDGE('',*,*,#8644,.T.);
#11421=ORIENTED_EDGE('',*,*,#8643,.F.);
#11422=ORIENTED_EDGE('',*,*,#8646,.T.);
#11423=ORIENTED_EDGE('',*,*,#8647,.T.);
#11424=ORIENTED_EDGE('',*,*,#8646,.F.);
#11425=ORIENTED_EDGE('',*,*,#8647,.F.);
#11426=ORIENTED_EDGE('',*,*,#8648,.F.);
#11427=ORIENTED_EDGE('',*,*,#8649,.T.);
#11428=ORIENTED_EDGE('',*,*,#8650,.F.);
#11429=ORIENTED_EDGE('',*,*,#8649,.F.);
#11430=ORIENTED_EDGE('',*,*,#8651,.F.);
#11431=ORIENTED_EDGE('',*,*,#8652,.T.);
#11432=ORIENTED_EDGE('',*,*,#8653,.F.);
#11433=ORIENTED_EDGE('',*,*,#8652,.F.);
#11434=ORIENTED_EDGE('',*,*,#8654,.F.);
#11435=ORIENTED_EDGE('',*,*,#8655,.T.);
#11436=ORIENTED_EDGE('',*,*,#8656,.F.);
#11437=ORIENTED_EDGE('',*,*,#8655,.F.);
#11438=ORIENTED_EDGE('',*,*,#8657,.F.);
#11439=ORIENTED_EDGE('',*,*,#8658,.T.);
#11440=ORIENTED_EDGE('',*,*,#8659,.F.);
#11441=ORIENTED_EDGE('',*,*,#8658,.F.);
#11442=ORIENTED_EDGE('',*,*,#8660,.F.);
#11443=ORIENTED_EDGE('',*,*,#8661,.T.);
#11444=ORIENTED_EDGE('',*,*,#8662,.F.);
#11445=ORIENTED_EDGE('',*,*,#8661,.F.);
#11446=ORIENTED_EDGE('',*,*,#8663,.F.);
#11447=ORIENTED_EDGE('',*,*,#8664,.F.);
#11448=ORIENTED_EDGE('',*,*,#8665,.F.);
#11449=ORIENTED_EDGE('',*,*,#8666,.T.);
#11450=ORIENTED_EDGE('',*,*,#8667,.F.);
#11451=ORIENTED_EDGE('',*,*,#8668,.T.);
#11452=ORIENTED_EDGE('',*,*,#8669,.F.);
#11453=ORIENTED_EDGE('',*,*,#8670,.F.);
#11454=ORIENTED_EDGE('',*,*,#8669,.T.);
#11455=ORIENTED_EDGE('',*,*,#8671,.T.);
#11456=ORIENTED_EDGE('',*,*,#8672,.T.);
#11457=ORIENTED_EDGE('',*,*,#8673,.F.);
#11458=ORIENTED_EDGE('',*,*,#8673,.T.);
#11459=ORIENTED_EDGE('',*,*,#8674,.T.);
#11460=ORIENTED_EDGE('',*,*,#8675,.T.);
#11461=ORIENTED_EDGE('',*,*,#8664,.T.);
#11462=ORIENTED_EDGE('',*,*,#8676,.T.);
#11463=ORIENTED_EDGE('',*,*,#8677,.T.);
#11464=ORIENTED_EDGE('',*,*,#8678,.T.);
#11465=ORIENTED_EDGE('',*,*,#8670,.T.);
#11466=ORIENTED_EDGE('',*,*,#8679,.T.);
#11467=ORIENTED_EDGE('',*,*,#8680,.T.);
#11468=ORIENTED_EDGE('',*,*,#8662,.T.);
#11469=ORIENTED_EDGE('',*,*,#8659,.T.);
#11470=ORIENTED_EDGE('',*,*,#8656,.T.);
#11471=ORIENTED_EDGE('',*,*,#8653,.T.);
#11472=ORIENTED_EDGE('',*,*,#8650,.T.);
#11473=ORIENTED_EDGE('',*,*,#8665,.T.);
#11474=ORIENTED_EDGE('',*,*,#8675,.F.);
#11475=ORIENTED_EDGE('',*,*,#8681,.T.);
#11476=ORIENTED_EDGE('',*,*,#8682,.T.);
#11477=ORIENTED_EDGE('',*,*,#8683,.F.);
#11478=ORIENTED_EDGE('',*,*,#8684,.T.);
#11479=ORIENTED_EDGE('',*,*,#8679,.F.);
#11480=ORIENTED_EDGE('',*,*,#8684,.F.);
#11481=ORIENTED_EDGE('',*,*,#8685,.F.);
#11482=ORIENTED_EDGE('',*,*,#8686,.T.);
#11483=ORIENTED_EDGE('',*,*,#8687,.F.);
#11484=ORIENTED_EDGE('',*,*,#8677,.F.);
#11485=ORIENTED_EDGE('',*,*,#8663,.T.);
#11486=ORIENTED_EDGE('',*,*,#8688,.T.);
#11487=ORIENTED_EDGE('',*,*,#8685,.T.);
#11488=ORIENTED_EDGE('',*,*,#8676,.F.);
#11489=ORIENTED_EDGE('',*,*,#8689,.F.);
#11490=ORIENTED_EDGE('',*,*,#8690,.T.);
#11491=ORIENTED_EDGE('',*,*,#8680,.F.);
#11492=ORIENTED_EDGE('',*,*,#8690,.F.);
#11493=ORIENTED_EDGE('',*,*,#8672,.F.);
#11494=ORIENTED_EDGE('',*,*,#8691,.T.);
#11495=ORIENTED_EDGE('',*,*,#8681,.F.);
#11496=ORIENTED_EDGE('',*,*,#8674,.F.);
#11497=ORIENTED_EDGE('',*,*,#8667,.T.);
#11498=ORIENTED_EDGE('',*,*,#8678,.F.);
#11499=ORIENTED_EDGE('',*,*,#8687,.T.);
#11500=ORIENTED_EDGE('',*,*,#8692,.T.);
#11501=ORIENTED_EDGE('',*,*,#8692,.F.);
#11502=ORIENTED_EDGE('',*,*,#8686,.F.);
#11503=ORIENTED_EDGE('',*,*,#8688,.F.);
#11504=ORIENTED_EDGE('',*,*,#8666,.F.);
#11505=ORIENTED_EDGE('',*,*,#8682,.F.);
#11506=ORIENTED_EDGE('',*,*,#8691,.F.);
#11507=ORIENTED_EDGE('',*,*,#8671,.F.);
#11508=ORIENTED_EDGE('',*,*,#8668,.F.);
#11509=ORIENTED_EDGE('',*,*,#8683,.T.);
#11510=ORIENTED_EDGE('',*,*,#8689,.T.);
#11511=ORIENTED_EDGE('',*,*,#8660,.T.);
#11512=ORIENTED_EDGE('',*,*,#8657,.T.);
#11513=ORIENTED_EDGE('',*,*,#8654,.T.);
#11514=ORIENTED_EDGE('',*,*,#8651,.T.);
#11515=ORIENTED_EDGE('',*,*,#8648,.T.);
#11516=ORIENTED_EDGE('',*,*,#8693,.F.);
#11517=ORIENTED_EDGE('',*,*,#8694,.T.);
#11518=ORIENTED_EDGE('',*,*,#8695,.T.);
#11519=ORIENTED_EDGE('',*,*,#8694,.F.);
#11520=ORIENTED_EDGE('',*,*,#8696,.F.);
#11521=ORIENTED_EDGE('',*,*,#8697,.T.);
#11522=ORIENTED_EDGE('',*,*,#8698,.T.);
#11523=ORIENTED_EDGE('',*,*,#8697,.F.);
#11524=ORIENTED_EDGE('',*,*,#8696,.T.);
#11525=ORIENTED_EDGE('',*,*,#8693,.T.);
#11526=ORIENTED_EDGE('',*,*,#8698,.F.);
#11527=ORIENTED_EDGE('',*,*,#8695,.F.);
#11528=ORIENTED_EDGE('',*,*,#8699,.F.);
#11529=ORIENTED_EDGE('',*,*,#8700,.T.);
#11530=ORIENTED_EDGE('',*,*,#8701,.T.);
#11531=ORIENTED_EDGE('',*,*,#8700,.F.);
#11532=ORIENTED_EDGE('',*,*,#8702,.F.);
#11533=ORIENTED_EDGE('',*,*,#8703,.T.);
#11534=ORIENTED_EDGE('',*,*,#8704,.T.);
#11535=ORIENTED_EDGE('',*,*,#8703,.F.);
#11536=ORIENTED_EDGE('',*,*,#8702,.T.);
#11537=ORIENTED_EDGE('',*,*,#8699,.T.);
#11538=ORIENTED_EDGE('',*,*,#8704,.F.);
#11539=ORIENTED_EDGE('',*,*,#8701,.F.);
#11540=ORIENTED_EDGE('',*,*,#8705,.F.);
#11541=ORIENTED_EDGE('',*,*,#8706,.T.);
#11542=ORIENTED_EDGE('',*,*,#8707,.F.);
#11543=ORIENTED_EDGE('',*,*,#8706,.F.);
#11544=ORIENTED_EDGE('',*,*,#8708,.F.);
#11545=ORIENTED_EDGE('',*,*,#8709,.T.);
#11546=ORIENTED_EDGE('',*,*,#8710,.F.);
#11547=ORIENTED_EDGE('',*,*,#8709,.F.);
#11548=ORIENTED_EDGE('',*,*,#8711,.F.);
#11549=ORIENTED_EDGE('',*,*,#8712,.T.);
#11550=ORIENTED_EDGE('',*,*,#8713,.F.);
#11551=ORIENTED_EDGE('',*,*,#8712,.F.);
#11552=ORIENTED_EDGE('',*,*,#8714,.F.);
#11553=ORIENTED_EDGE('',*,*,#8715,.T.);
#11554=ORIENTED_EDGE('',*,*,#8716,.F.);
#11555=ORIENTED_EDGE('',*,*,#8715,.F.);
#11556=ORIENTED_EDGE('',*,*,#8717,.F.);
#11557=ORIENTED_EDGE('',*,*,#8718,.T.);
#11558=ORIENTED_EDGE('',*,*,#8719,.T.);
#11559=ORIENTED_EDGE('',*,*,#8718,.F.);
#11560=ORIENTED_EDGE('',*,*,#8720,.F.);
#11561=ORIENTED_EDGE('',*,*,#8721,.T.);
#11562=ORIENTED_EDGE('',*,*,#8722,.T.);
#11563=ORIENTED_EDGE('',*,*,#8721,.F.);
#11564=ORIENTED_EDGE('',*,*,#8720,.T.);
#11565=ORIENTED_EDGE('',*,*,#8717,.T.);
#11566=ORIENTED_EDGE('',*,*,#8716,.T.);
#11567=ORIENTED_EDGE('',*,*,#8713,.T.);
#11568=ORIENTED_EDGE('',*,*,#8710,.T.);
#11569=ORIENTED_EDGE('',*,*,#8707,.T.);
#11570=ORIENTED_EDGE('',*,*,#8722,.F.);
#11571=ORIENTED_EDGE('',*,*,#8719,.F.);
#11572=ORIENTED_EDGE('',*,*,#8714,.T.);
#11573=ORIENTED_EDGE('',*,*,#8711,.T.);
#11574=ORIENTED_EDGE('',*,*,#8708,.T.);
#11575=ORIENTED_EDGE('',*,*,#8705,.T.);
#11576=ORIENTED_EDGE('',*,*,#8723,.T.);
#11577=ORIENTED_EDGE('',*,*,#8724,.F.);
#11578=ORIENTED_EDGE('',*,*,#8723,.F.);
#11579=ORIENTED_EDGE('',*,*,#8725,.T.);
#11580=ORIENTED_EDGE('',*,*,#8726,.T.);
#11581=ORIENTED_EDGE('',*,*,#8725,.F.);
#11582=ORIENTED_EDGE('',*,*,#8726,.F.);
#11583=ORIENTED_EDGE('',*,*,#8727,.F.);
#11584=ORIENTED_EDGE('',*,*,#8728,.T.);
#11585=ORIENTED_EDGE('',*,*,#8724,.T.);
#11586=ORIENTED_EDGE('',*,*,#8728,.F.);
#11587=ORIENTED_EDGE('',*,*,#8727,.T.);
#11588=ORIENTED_EDGE('',*,*,#8729,.T.);
#11589=ORIENTED_EDGE('',*,*,#8730,.F.);
#11590=ORIENTED_EDGE('',*,*,#8729,.F.);
#11591=ORIENTED_EDGE('',*,*,#8731,.T.);
#11592=ORIENTED_EDGE('',*,*,#8732,.T.);
#11593=ORIENTED_EDGE('',*,*,#8731,.F.);
#11594=ORIENTED_EDGE('',*,*,#8732,.F.);
#11595=ORIENTED_EDGE('',*,*,#8733,.F.);
#11596=ORIENTED_EDGE('',*,*,#8734,.T.);
#11597=ORIENTED_EDGE('',*,*,#8730,.T.);
#11598=ORIENTED_EDGE('',*,*,#8734,.F.);
#11599=ORIENTED_EDGE('',*,*,#8733,.T.);
#11600=ORIENTED_EDGE('',*,*,#8735,.T.);
#11601=ORIENTED_EDGE('',*,*,#8736,.F.);
#11602=ORIENTED_EDGE('',*,*,#8735,.F.);
#11603=ORIENTED_EDGE('',*,*,#8737,.T.);
#11604=ORIENTED_EDGE('',*,*,#8738,.T.);
#11605=ORIENTED_EDGE('',*,*,#8737,.F.);
#11606=ORIENTED_EDGE('',*,*,#8738,.F.);
#11607=ORIENTED_EDGE('',*,*,#8739,.F.);
#11608=ORIENTED_EDGE('',*,*,#8740,.T.);
#11609=ORIENTED_EDGE('',*,*,#8736,.T.);
#11610=ORIENTED_EDGE('',*,*,#8740,.F.);
#11611=ORIENTED_EDGE('',*,*,#8739,.T.);
#11612=ORIENTED_EDGE('',*,*,#8741,.T.);
#11613=ORIENTED_EDGE('',*,*,#8742,.F.);
#11614=ORIENTED_EDGE('',*,*,#8741,.F.);
#11615=ORIENTED_EDGE('',*,*,#8743,.T.);
#11616=ORIENTED_EDGE('',*,*,#8744,.T.);
#11617=ORIENTED_EDGE('',*,*,#8743,.F.);
#11618=ORIENTED_EDGE('',*,*,#8744,.F.);
#11619=ORIENTED_EDGE('',*,*,#8745,.F.);
#11620=ORIENTED_EDGE('',*,*,#8746,.T.);
#11621=ORIENTED_EDGE('',*,*,#8742,.T.);
#11622=ORIENTED_EDGE('',*,*,#8746,.F.);
#11623=ORIENTED_EDGE('',*,*,#8745,.T.);
#11624=ORIENTED_EDGE('',*,*,#8747,.F.);
#11625=ORIENTED_EDGE('',*,*,#8748,.T.);
#11626=ORIENTED_EDGE('',*,*,#8749,.F.);
#11627=ORIENTED_EDGE('',*,*,#8748,.F.);
#11628=ORIENTED_EDGE('',*,*,#8750,.F.);
#11629=ORIENTED_EDGE('',*,*,#8751,.T.);
#11630=ORIENTED_EDGE('',*,*,#8752,.F.);
#11631=ORIENTED_EDGE('',*,*,#8751,.F.);
#11632=ORIENTED_EDGE('',*,*,#8753,.F.);
#11633=ORIENTED_EDGE('',*,*,#8754,.T.);
#11634=ORIENTED_EDGE('',*,*,#8755,.F.);
#11635=ORIENTED_EDGE('',*,*,#8754,.F.);
#11636=ORIENTED_EDGE('',*,*,#8756,.F.);
#11637=ORIENTED_EDGE('',*,*,#8757,.T.);
#11638=ORIENTED_EDGE('',*,*,#8758,.F.);
#11639=ORIENTED_EDGE('',*,*,#8757,.F.);
#11640=ORIENTED_EDGE('',*,*,#8759,.F.);
#11641=ORIENTED_EDGE('',*,*,#8760,.T.);
#11642=ORIENTED_EDGE('',*,*,#8761,.T.);
#11643=ORIENTED_EDGE('',*,*,#8760,.F.);
#11644=ORIENTED_EDGE('',*,*,#8762,.F.);
#11645=ORIENTED_EDGE('',*,*,#8763,.T.);
#11646=ORIENTED_EDGE('',*,*,#8764,.T.);
#11647=ORIENTED_EDGE('',*,*,#8763,.F.);
#11648=ORIENTED_EDGE('',*,*,#8762,.T.);
#11649=ORIENTED_EDGE('',*,*,#8759,.T.);
#11650=ORIENTED_EDGE('',*,*,#8758,.T.);
#11651=ORIENTED_EDGE('',*,*,#8755,.T.);
#11652=ORIENTED_EDGE('',*,*,#8752,.T.);
#11653=ORIENTED_EDGE('',*,*,#8749,.T.);
#11654=ORIENTED_EDGE('',*,*,#8764,.F.);
#11655=ORIENTED_EDGE('',*,*,#8761,.F.);
#11656=ORIENTED_EDGE('',*,*,#8756,.T.);
#11657=ORIENTED_EDGE('',*,*,#8753,.T.);
#11658=ORIENTED_EDGE('',*,*,#8750,.T.);
#11659=ORIENTED_EDGE('',*,*,#8747,.T.);
#11660=ORIENTED_EDGE('',*,*,#8765,.F.);
#11661=ORIENTED_EDGE('',*,*,#8766,.T.);
#11662=ORIENTED_EDGE('',*,*,#8767,.F.);
#11663=ORIENTED_EDGE('',*,*,#8768,.T.);
#11664=ORIENTED_EDGE('',*,*,#8765,.T.);
#11665=ORIENTED_EDGE('',*,*,#8768,.F.);
#11666=ORIENTED_EDGE('',*,*,#8767,.T.);
#11667=ORIENTED_EDGE('',*,*,#8766,.F.);
#11668=ORIENTED_EDGE('',*,*,#8769,.T.);
#11669=ORIENTED_EDGE('',*,*,#8770,.T.);
#11670=ORIENTED_EDGE('',*,*,#8769,.F.);
#11671=ORIENTED_EDGE('',*,*,#8770,.F.);
#11672=ORIENTED_EDGE('',*,*,#8771,.F.);
#11673=ORIENTED_EDGE('',*,*,#8772,.T.);
#11674=ORIENTED_EDGE('',*,*,#8773,.F.);
#11675=ORIENTED_EDGE('',*,*,#8774,.T.);
#11676=ORIENTED_EDGE('',*,*,#8771,.T.);
#11677=ORIENTED_EDGE('',*,*,#8774,.F.);
#11678=ORIENTED_EDGE('',*,*,#8773,.T.);
#11679=ORIENTED_EDGE('',*,*,#8772,.F.);
#11680=ORIENTED_EDGE('',*,*,#8775,.T.);
#11681=ORIENTED_EDGE('',*,*,#8776,.T.);
#11682=ORIENTED_EDGE('',*,*,#8775,.F.);
#11683=ORIENTED_EDGE('',*,*,#8776,.F.);
#11684=ORIENTED_EDGE('',*,*,#8777,.F.);
#11685=ORIENTED_EDGE('',*,*,#8778,.T.);
#11686=ORIENTED_EDGE('',*,*,#8779,.F.);
#11687=ORIENTED_EDGE('',*,*,#8780,.T.);
#11688=ORIENTED_EDGE('',*,*,#8777,.T.);
#11689=ORIENTED_EDGE('',*,*,#8780,.F.);
#11690=ORIENTED_EDGE('',*,*,#8779,.T.);
#11691=ORIENTED_EDGE('',*,*,#8778,.F.);
#11692=ORIENTED_EDGE('',*,*,#8781,.T.);
#11693=ORIENTED_EDGE('',*,*,#8782,.T.);
#11694=ORIENTED_EDGE('',*,*,#8781,.F.);
#11695=ORIENTED_EDGE('',*,*,#8782,.F.);
#11696=ORIENTED_EDGE('',*,*,#8783,.F.);
#11697=ORIENTED_EDGE('',*,*,#8784,.T.);
#11698=ORIENTED_EDGE('',*,*,#8785,.F.);
#11699=ORIENTED_EDGE('',*,*,#8786,.T.);
#11700=ORIENTED_EDGE('',*,*,#8783,.T.);
#11701=ORIENTED_EDGE('',*,*,#8786,.F.);
#11702=ORIENTED_EDGE('',*,*,#8785,.T.);
#11703=ORIENTED_EDGE('',*,*,#8784,.F.);
#11704=ORIENTED_EDGE('',*,*,#8787,.T.);
#11705=ORIENTED_EDGE('',*,*,#8788,.T.);
#11706=ORIENTED_EDGE('',*,*,#8787,.F.);
#11707=ORIENTED_EDGE('',*,*,#8788,.F.);
#11708=ORIENTED_EDGE('',*,*,#8789,.F.);
#11709=ORIENTED_EDGE('',*,*,#8790,.F.);
#11710=ORIENTED_EDGE('',*,*,#8791,.T.);
#11711=ORIENTED_EDGE('',*,*,#8792,.F.);
#11712=ORIENTED_EDGE('',*,*,#8793,.F.);
#11713=ORIENTED_EDGE('',*,*,#8791,.F.);
#11714=ORIENTED_EDGE('',*,*,#8792,.T.);
#11715=ORIENTED_EDGE('',*,*,#8793,.T.);
#11716=ORIENTED_EDGE('',*,*,#8794,.T.);
#11717=ORIENTED_EDGE('',*,*,#8795,.T.);
#11718=ORIENTED_EDGE('',*,*,#8794,.F.);
#11719=ORIENTED_EDGE('',*,*,#8796,.T.);
#11720=ORIENTED_EDGE('',*,*,#8797,.T.);
#11721=ORIENTED_EDGE('',*,*,#8798,.F.);
#11722=ORIENTED_EDGE('',*,*,#8797,.F.);
#11723=ORIENTED_EDGE('',*,*,#8798,.T.);
#11724=ORIENTED_EDGE('',*,*,#8799,.T.);
#11725=ORIENTED_EDGE('',*,*,#8800,.F.);
#11726=ORIENTED_EDGE('',*,*,#8799,.F.);
#11727=ORIENTED_EDGE('',*,*,#8795,.F.);
#11728=ORIENTED_EDGE('',*,*,#8800,.T.);
#11729=ORIENTED_EDGE('',*,*,#8801,.F.);
#11730=ORIENTED_EDGE('',*,*,#8802,.T.);
#11731=ORIENTED_EDGE('',*,*,#8789,.T.);
#11732=ORIENTED_EDGE('',*,*,#8790,.T.);
#11733=ORIENTED_EDGE('',*,*,#8802,.F.);
#11734=ORIENTED_EDGE('',*,*,#8801,.T.);
#11735=ORIENTED_EDGE('',*,*,#8803,.F.);
#11736=ORIENTED_EDGE('',*,*,#8803,.T.);
#11737=ORIENTED_EDGE('',*,*,#8804,.T.);
#11738=ORIENTED_EDGE('',*,*,#8796,.F.);
#11739=ORIENTED_EDGE('',*,*,#8804,.F.);
#11740=ORIENTED_EDGE('',*,*,#8805,.F.);
#11741=ORIENTED_EDGE('',*,*,#8806,.F.);
#11742=ORIENTED_EDGE('',*,*,#8807,.T.);
#11743=ORIENTED_EDGE('',*,*,#8808,.F.);
#11744=ORIENTED_EDGE('',*,*,#8809,.F.);
#11745=ORIENTED_EDGE('',*,*,#8807,.F.);
#11746=ORIENTED_EDGE('',*,*,#8810,.T.);
#11747=ORIENTED_EDGE('',*,*,#8811,.T.);
#11748=ORIENTED_EDGE('',*,*,#8808,.T.);
#11749=ORIENTED_EDGE('',*,*,#8809,.T.);
#11750=ORIENTED_EDGE('',*,*,#8811,.F.);
#11751=ORIENTED_EDGE('',*,*,#8812,.F.);
#11752=ORIENTED_EDGE('',*,*,#8813,.T.);
#11753=ORIENTED_EDGE('',*,*,#8814,.F.);
#11754=ORIENTED_EDGE('',*,*,#8815,.T.);
#11755=ORIENTED_EDGE('',*,*,#8812,.T.);
#11756=ORIENTED_EDGE('',*,*,#8815,.F.);
#11757=ORIENTED_EDGE('',*,*,#8816,.F.);
#11758=ORIENTED_EDGE('',*,*,#8817,.T.);
#11759=ORIENTED_EDGE('',*,*,#8814,.T.);
#11760=ORIENTED_EDGE('',*,*,#8817,.F.);
#11761=ORIENTED_EDGE('',*,*,#8818,.F.);
#11762=ORIENTED_EDGE('',*,*,#8819,.T.);
#11763=ORIENTED_EDGE('',*,*,#8816,.T.);
#11764=ORIENTED_EDGE('',*,*,#8819,.F.);
#11765=ORIENTED_EDGE('',*,*,#8818,.T.);
#11766=ORIENTED_EDGE('',*,*,#8810,.F.);
#11767=ORIENTED_EDGE('',*,*,#8805,.T.);
#11768=ORIENTED_EDGE('',*,*,#8806,.T.);
#11769=ORIENTED_EDGE('',*,*,#8820,.T.);
#11770=ORIENTED_EDGE('',*,*,#8813,.F.);
#11771=ORIENTED_EDGE('',*,*,#8820,.F.);
#11772=ORIENTED_EDGE('',*,*,#8821,.T.);
#11773=ORIENTED_EDGE('',*,*,#8821,.F.);
#11774=ORIENTED_EDGE('',*,*,#8822,.T.);
#11775=ORIENTED_EDGE('',*,*,#8822,.F.);
#11776=ORIENTED_EDGE('',*,*,#8823,.T.);
#11777=ORIENTED_EDGE('',*,*,#8823,.F.);
#11778=ORIENTED_EDGE('',*,*,#8824,.T.);
#11779=ORIENTED_EDGE('',*,*,#8824,.F.);
#11780=ORIENTED_EDGE('',*,*,#8825,.T.);
#11781=ORIENTED_EDGE('',*,*,#8825,.F.);
#11782=ORIENTED_EDGE('',*,*,#8826,.T.);
#11783=ORIENTED_EDGE('',*,*,#8826,.F.);
#11784=ORIENTED_EDGE('',*,*,#8827,.T.);
#11785=ORIENTED_EDGE('',*,*,#8827,.F.);
#11786=ORIENTED_EDGE('',*,*,#8828,.F.);
#11787=ORIENTED_EDGE('',*,*,#8829,.F.);
#11788=ORIENTED_EDGE('',*,*,#8830,.F.);
#11789=ORIENTED_EDGE('',*,*,#8831,.F.);
#11790=ORIENTED_EDGE('',*,*,#8831,.T.);
#11791=ORIENTED_EDGE('',*,*,#8832,.T.);
#11792=ORIENTED_EDGE('',*,*,#8833,.T.);
#11793=ORIENTED_EDGE('',*,*,#8834,.F.);
#11794=ORIENTED_EDGE('',*,*,#8830,.T.);
#11795=ORIENTED_EDGE('',*,*,#8835,.T.);
#11796=ORIENTED_EDGE('',*,*,#8836,.T.);
#11797=ORIENTED_EDGE('',*,*,#8832,.F.);
#11798=ORIENTED_EDGE('',*,*,#8829,.T.);
#11799=ORIENTED_EDGE('',*,*,#8837,.T.);
#11800=ORIENTED_EDGE('',*,*,#8838,.T.);
#11801=ORIENTED_EDGE('',*,*,#8835,.F.);
#11802=ORIENTED_EDGE('',*,*,#8828,.T.);
#11803=ORIENTED_EDGE('',*,*,#8834,.T.);
#11804=ORIENTED_EDGE('',*,*,#8839,.T.);
#11805=ORIENTED_EDGE('',*,*,#8837,.F.);
#11806=ORIENTED_EDGE('',*,*,#8833,.F.);
#11807=ORIENTED_EDGE('',*,*,#8836,.F.);
#11808=ORIENTED_EDGE('',*,*,#8838,.F.);
#11809=ORIENTED_EDGE('',*,*,#8839,.F.);
#11810=ORIENTED_EDGE('',*,*,#8840,.F.);
#11811=ORIENTED_EDGE('',*,*,#8841,.F.);
#11812=ORIENTED_EDGE('',*,*,#8842,.F.);
#11813=ORIENTED_EDGE('',*,*,#8843,.F.);
#11814=ORIENTED_EDGE('',*,*,#8842,.T.);
#11815=ORIENTED_EDGE('',*,*,#8844,.T.);
#11816=ORIENTED_EDGE('',*,*,#8845,.T.);
#11817=ORIENTED_EDGE('',*,*,#8846,.F.);
#11818=ORIENTED_EDGE('',*,*,#8843,.T.);
#11819=ORIENTED_EDGE('',*,*,#8846,.T.);
#11820=ORIENTED_EDGE('',*,*,#8847,.T.);
#11821=ORIENTED_EDGE('',*,*,#8848,.F.);
#11822=ORIENTED_EDGE('',*,*,#8841,.T.);
#11823=ORIENTED_EDGE('',*,*,#8849,.T.);
#11824=ORIENTED_EDGE('',*,*,#8850,.T.);
#11825=ORIENTED_EDGE('',*,*,#8844,.F.);
#11826=ORIENTED_EDGE('',*,*,#8840,.T.);
#11827=ORIENTED_EDGE('',*,*,#8848,.T.);
#11828=ORIENTED_EDGE('',*,*,#8851,.T.);
#11829=ORIENTED_EDGE('',*,*,#8849,.F.);
#11830=ORIENTED_EDGE('',*,*,#8845,.F.);
#11831=ORIENTED_EDGE('',*,*,#8850,.F.);
#11832=ORIENTED_EDGE('',*,*,#8851,.F.);
#11833=ORIENTED_EDGE('',*,*,#8847,.F.);
#11834=ORIENTED_EDGE('',*,*,#8852,.F.);
#11835=ORIENTED_EDGE('',*,*,#8853,.F.);
#11836=ORIENTED_EDGE('',*,*,#8854,.F.);
#11837=ORIENTED_EDGE('',*,*,#8855,.F.);
#11838=ORIENTED_EDGE('',*,*,#8854,.T.);
#11839=ORIENTED_EDGE('',*,*,#8856,.T.);
#11840=ORIENTED_EDGE('',*,*,#8857,.T.);
#11841=ORIENTED_EDGE('',*,*,#8858,.F.);
#11842=ORIENTED_EDGE('',*,*,#8855,.T.);
#11843=ORIENTED_EDGE('',*,*,#8858,.T.);
#11844=ORIENTED_EDGE('',*,*,#8859,.T.);
#11845=ORIENTED_EDGE('',*,*,#8860,.F.);
#11846=ORIENTED_EDGE('',*,*,#8853,.T.);
#11847=ORIENTED_EDGE('',*,*,#8861,.T.);
#11848=ORIENTED_EDGE('',*,*,#8862,.T.);
#11849=ORIENTED_EDGE('',*,*,#8856,.F.);
#11850=ORIENTED_EDGE('',*,*,#8852,.T.);
#11851=ORIENTED_EDGE('',*,*,#8860,.T.);
#11852=ORIENTED_EDGE('',*,*,#8863,.T.);
#11853=ORIENTED_EDGE('',*,*,#8861,.F.);
#11854=ORIENTED_EDGE('',*,*,#8859,.F.);
#11855=ORIENTED_EDGE('',*,*,#8857,.F.);
#11856=ORIENTED_EDGE('',*,*,#8862,.F.);
#11857=ORIENTED_EDGE('',*,*,#8863,.F.);
#11858=ORIENTED_EDGE('',*,*,#8864,.F.);
#11859=ORIENTED_EDGE('',*,*,#8865,.F.);
#11860=ORIENTED_EDGE('',*,*,#8866,.F.);
#11861=ORIENTED_EDGE('',*,*,#8867,.F.);
#11862=ORIENTED_EDGE('',*,*,#8867,.T.);
#11863=ORIENTED_EDGE('',*,*,#8868,.F.);
#11864=ORIENTED_EDGE('',*,*,#8869,.T.);
#11865=ORIENTED_EDGE('',*,*,#8870,.T.);
#11866=ORIENTED_EDGE('',*,*,#8866,.T.);
#11867=ORIENTED_EDGE('',*,*,#8871,.F.);
#11868=ORIENTED_EDGE('',*,*,#8872,.T.);
#11869=ORIENTED_EDGE('',*,*,#8868,.T.);
#11870=ORIENTED_EDGE('',*,*,#8865,.T.);
#11871=ORIENTED_EDGE('',*,*,#8873,.F.);
#11872=ORIENTED_EDGE('',*,*,#8874,.T.);
#11873=ORIENTED_EDGE('',*,*,#8871,.T.);
#11874=ORIENTED_EDGE('',*,*,#8864,.T.);
#11875=ORIENTED_EDGE('',*,*,#8870,.F.);
#11876=ORIENTED_EDGE('',*,*,#8875,.T.);
#11877=ORIENTED_EDGE('',*,*,#8873,.T.);
#11878=ORIENTED_EDGE('',*,*,#8875,.F.);
#11879=ORIENTED_EDGE('',*,*,#8869,.F.);
#11880=ORIENTED_EDGE('',*,*,#8872,.F.);
#11881=ORIENTED_EDGE('',*,*,#8874,.F.);
#11882=ORIENTED_EDGE('',*,*,#8876,.F.);
#11883=ORIENTED_EDGE('',*,*,#8877,.F.);
#11884=ORIENTED_EDGE('',*,*,#8878,.F.);
#11885=ORIENTED_EDGE('',*,*,#8879,.F.);
#11886=ORIENTED_EDGE('',*,*,#8880,.T.);
#11887=ORIENTED_EDGE('',*,*,#8881,.T.);
#11888=ORIENTED_EDGE('',*,*,#8876,.T.);
#11889=ORIENTED_EDGE('',*,*,#8882,.F.);
#11890=ORIENTED_EDGE('',*,*,#8883,.T.);
#11891=ORIENTED_EDGE('',*,*,#8882,.T.);
#11892=ORIENTED_EDGE('',*,*,#8879,.T.);
#11893=ORIENTED_EDGE('',*,*,#8884,.F.);
#11894=ORIENTED_EDGE('',*,*,#8885,.T.);
#11895=ORIENTED_EDGE('',*,*,#8886,.T.);
#11896=ORIENTED_EDGE('',*,*,#8877,.T.);
#11897=ORIENTED_EDGE('',*,*,#8881,.F.);
#11898=ORIENTED_EDGE('',*,*,#8887,.T.);
#11899=ORIENTED_EDGE('',*,*,#8884,.T.);
#11900=ORIENTED_EDGE('',*,*,#8878,.T.);
#11901=ORIENTED_EDGE('',*,*,#8886,.F.);
#11902=ORIENTED_EDGE('',*,*,#8883,.F.);
#11903=ORIENTED_EDGE('',*,*,#8887,.F.);
#11904=ORIENTED_EDGE('',*,*,#8885,.F.);
#11905=ORIENTED_EDGE('',*,*,#8880,.F.);
#11906=ORIENTED_EDGE('',*,*,#8888,.F.);
#11907=ORIENTED_EDGE('',*,*,#8889,.F.);
#11908=ORIENTED_EDGE('',*,*,#8890,.F.);
#11909=ORIENTED_EDGE('',*,*,#8891,.F.);
#11910=ORIENTED_EDGE('',*,*,#8892,.T.);
#11911=ORIENTED_EDGE('',*,*,#8893,.T.);
#11912=ORIENTED_EDGE('',*,*,#8888,.T.);
#11913=ORIENTED_EDGE('',*,*,#8894,.F.);
#11914=ORIENTED_EDGE('',*,*,#8895,.T.);
#11915=ORIENTED_EDGE('',*,*,#8894,.T.);
#11916=ORIENTED_EDGE('',*,*,#8891,.T.);
#11917=ORIENTED_EDGE('',*,*,#8896,.F.);
#11918=ORIENTED_EDGE('',*,*,#8897,.T.);
#11919=ORIENTED_EDGE('',*,*,#8896,.T.);
#11920=ORIENTED_EDGE('',*,*,#8890,.T.);
#11921=ORIENTED_EDGE('',*,*,#8898,.F.);
#11922=ORIENTED_EDGE('',*,*,#8899,.T.);
#11923=ORIENTED_EDGE('',*,*,#8898,.T.);
#11924=ORIENTED_EDGE('',*,*,#8889,.T.);
#11925=ORIENTED_EDGE('',*,*,#8893,.F.);
#11926=ORIENTED_EDGE('',*,*,#8895,.F.);
#11927=ORIENTED_EDGE('',*,*,#8897,.F.);
#11928=ORIENTED_EDGE('',*,*,#8899,.F.);
#11929=ORIENTED_EDGE('',*,*,#8892,.F.);
#11930=ORIENTED_EDGE('',*,*,#8900,.T.);
#11931=ORIENTED_EDGE('',*,*,#8901,.T.);
#11932=ORIENTED_EDGE('',*,*,#8902,.T.);
#11933=ORIENTED_EDGE('',*,*,#8903,.F.);
#11934=ORIENTED_EDGE('',*,*,#8904,.T.);
#11935=ORIENTED_EDGE('',*,*,#8903,.T.);
#11936=ORIENTED_EDGE('',*,*,#8905,.T.);
#11937=ORIENTED_EDGE('',*,*,#8906,.F.);
#11938=ORIENTED_EDGE('',*,*,#8907,.F.);
#11939=ORIENTED_EDGE('',*,*,#8908,.F.);
#11940=ORIENTED_EDGE('',*,*,#8905,.F.);
#11941=ORIENTED_EDGE('',*,*,#8902,.F.);
#11942=ORIENTED_EDGE('',*,*,#8909,.T.);
#11943=ORIENTED_EDGE('',*,*,#8910,.T.);
#11944=ORIENTED_EDGE('',*,*,#8907,.T.);
#11945=ORIENTED_EDGE('',*,*,#8901,.F.);
#11946=ORIENTED_EDGE('',*,*,#8911,.T.);
#11947=ORIENTED_EDGE('',*,*,#8906,.T.);
#11948=ORIENTED_EDGE('',*,*,#8908,.T.);
#11949=ORIENTED_EDGE('',*,*,#8910,.F.);
#11950=ORIENTED_EDGE('',*,*,#8904,.F.);
#11951=ORIENTED_EDGE('',*,*,#8911,.F.);
#11952=ORIENTED_EDGE('',*,*,#8909,.F.);
#11953=ORIENTED_EDGE('',*,*,#8900,.F.);
#11954=ORIENTED_EDGE('',*,*,#8912,.F.);
#11955=ORIENTED_EDGE('',*,*,#8913,.T.);
#11956=ORIENTED_EDGE('',*,*,#8914,.F.);
#11957=ORIENTED_EDGE('',*,*,#8915,.T.);
#11958=ORIENTED_EDGE('',*,*,#8912,.T.);
#11959=ORIENTED_EDGE('',*,*,#8915,.F.);
#11960=ORIENTED_EDGE('',*,*,#8914,.T.);
#11961=ORIENTED_EDGE('',*,*,#8916,.F.);
#11962=ORIENTED_EDGE('',*,*,#8916,.T.);
#11963=ORIENTED_EDGE('',*,*,#8917,.T.);
#11964=ORIENTED_EDGE('',*,*,#8913,.F.);
#11965=ORIENTED_EDGE('',*,*,#8917,.F.);
#11966=ORIENTED_EDGE('',*,*,#8918,.F.);
#11967=ORIENTED_EDGE('',*,*,#8919,.T.);
#11968=ORIENTED_EDGE('',*,*,#8920,.F.);
#11969=ORIENTED_EDGE('',*,*,#8921,.T.);
#11970=ORIENTED_EDGE('',*,*,#8918,.T.);
#11971=ORIENTED_EDGE('',*,*,#8921,.F.);
#11972=ORIENTED_EDGE('',*,*,#8920,.T.);
#11973=ORIENTED_EDGE('',*,*,#8922,.F.);
#11974=ORIENTED_EDGE('',*,*,#8922,.T.);
#11975=ORIENTED_EDGE('',*,*,#8923,.T.);
#11976=ORIENTED_EDGE('',*,*,#8919,.F.);
#11977=ORIENTED_EDGE('',*,*,#8923,.F.);
#11978=ORIENTED_EDGE('',*,*,#8924,.T.);
#11979=ORIENTED_EDGE('',*,*,#8925,.F.);
#11980=ORIENTED_EDGE('',*,*,#8926,.F.);
#11981=ORIENTED_EDGE('',*,*,#8927,.F.);
#11982=ORIENTED_EDGE('',*,*,#8924,.F.);
#11983=ORIENTED_EDGE('',*,*,#8928,.T.);
#11984=ORIENTED_EDGE('',*,*,#8926,.T.);
#11985=ORIENTED_EDGE('',*,*,#8928,.F.);
#11986=ORIENTED_EDGE('',*,*,#8927,.T.);
#11987=ORIENTED_EDGE('',*,*,#8929,.T.);
#11988=ORIENTED_EDGE('',*,*,#8930,.T.);
#11989=ORIENTED_EDGE('',*,*,#8929,.F.);
#11990=ORIENTED_EDGE('',*,*,#8931,.T.);
#11991=ORIENTED_EDGE('',*,*,#8930,.F.);
#11992=ORIENTED_EDGE('',*,*,#8932,.F.);
#11993=ORIENTED_EDGE('',*,*,#8933,.F.);
#11994=ORIENTED_EDGE('',*,*,#8931,.F.);
#11995=ORIENTED_EDGE('',*,*,#8934,.T.);
#11996=ORIENTED_EDGE('',*,*,#8932,.T.);
#11997=ORIENTED_EDGE('',*,*,#8934,.F.);
#11998=ORIENTED_EDGE('',*,*,#8933,.T.);
#11999=ORIENTED_EDGE('',*,*,#8935,.T.);
#12000=ORIENTED_EDGE('',*,*,#8936,.T.);
#12001=ORIENTED_EDGE('',*,*,#8935,.F.);
#12002=ORIENTED_EDGE('',*,*,#8937,.F.);
#12003=ORIENTED_EDGE('',*,*,#8938,.T.);
#12004=ORIENTED_EDGE('',*,*,#8925,.T.);
#12005=ORIENTED_EDGE('',*,*,#8938,.F.);
#12006=ORIENTED_EDGE('',*,*,#8937,.T.);
#12007=ORIENTED_EDGE('',*,*,#8936,.F.);
#12008=ORIENTED_EDGE('',*,*,#8939,.F.);
#12009=ORIENTED_EDGE('',*,*,#8940,.T.);
#12010=ORIENTED_EDGE('',*,*,#8941,.T.);
#12011=ORIENTED_EDGE('',*,*,#8940,.F.);
#12012=ORIENTED_EDGE('',*,*,#8942,.F.);
#12013=ORIENTED_EDGE('',*,*,#8943,.T.);
#12014=ORIENTED_EDGE('',*,*,#8944,.T.);
#12015=ORIENTED_EDGE('',*,*,#8943,.F.);
#12016=ORIENTED_EDGE('',*,*,#8942,.T.);
#12017=ORIENTED_EDGE('',*,*,#8939,.T.);
#12018=ORIENTED_EDGE('',*,*,#8944,.F.);
#12019=ORIENTED_EDGE('',*,*,#8941,.F.);
#12020=ORIENTED_EDGE('',*,*,#8945,.F.);
#12021=ORIENTED_EDGE('',*,*,#8946,.T.);
#12022=ORIENTED_EDGE('',*,*,#8947,.T.);
#12023=ORIENTED_EDGE('',*,*,#8946,.F.);
#12024=ORIENTED_EDGE('',*,*,#8948,.F.);
#12025=ORIENTED_EDGE('',*,*,#8949,.T.);
#12026=ORIENTED_EDGE('',*,*,#8950,.T.);
#12027=ORIENTED_EDGE('',*,*,#8949,.F.);
#12028=ORIENTED_EDGE('',*,*,#8948,.T.);
#12029=ORIENTED_EDGE('',*,*,#8945,.T.);
#12030=ORIENTED_EDGE('',*,*,#8950,.F.);
#12031=ORIENTED_EDGE('',*,*,#8947,.F.);
#12032=ORIENTED_EDGE('',*,*,#8951,.F.);
#12033=ORIENTED_EDGE('',*,*,#8952,.T.);
#12034=ORIENTED_EDGE('',*,*,#8953,.T.);
#12035=ORIENTED_EDGE('',*,*,#8952,.F.);
#12036=ORIENTED_EDGE('',*,*,#8954,.F.);
#12037=ORIENTED_EDGE('',*,*,#8955,.T.);
#12038=ORIENTED_EDGE('',*,*,#8956,.T.);
#12039=ORIENTED_EDGE('',*,*,#8955,.F.);
#12040=ORIENTED_EDGE('',*,*,#8954,.T.);
#12041=ORIENTED_EDGE('',*,*,#8951,.T.);
#12042=ORIENTED_EDGE('',*,*,#8956,.F.);
#12043=ORIENTED_EDGE('',*,*,#8953,.F.);
#12044=ORIENTED_EDGE('',*,*,#8957,.F.);
#12045=ORIENTED_EDGE('',*,*,#8958,.T.);
#12046=ORIENTED_EDGE('',*,*,#8959,.T.);
#12047=ORIENTED_EDGE('',*,*,#8958,.F.);
#12048=ORIENTED_EDGE('',*,*,#8960,.F.);
#12049=ORIENTED_EDGE('',*,*,#8961,.T.);
#12050=ORIENTED_EDGE('',*,*,#8962,.T.);
#12051=ORIENTED_EDGE('',*,*,#8961,.F.);
#12052=ORIENTED_EDGE('',*,*,#8960,.T.);
#12053=ORIENTED_EDGE('',*,*,#8957,.T.);
#12054=ORIENTED_EDGE('',*,*,#8962,.F.);
#12055=ORIENTED_EDGE('',*,*,#8959,.F.);
#12056=ORIENTED_EDGE('',*,*,#8963,.F.);
#12057=ORIENTED_EDGE('',*,*,#8964,.T.);
#12058=ORIENTED_EDGE('',*,*,#8965,.T.);
#12059=ORIENTED_EDGE('',*,*,#8964,.F.);
#12060=ORIENTED_EDGE('',*,*,#8965,.F.);
#12061=ORIENTED_EDGE('',*,*,#8966,.F.);
#12062=ORIENTED_EDGE('',*,*,#8967,.T.);
#12063=ORIENTED_EDGE('',*,*,#8968,.T.);
#12064=ORIENTED_EDGE('',*,*,#8967,.F.);
#12065=ORIENTED_EDGE('',*,*,#8969,.F.);
#12066=ORIENTED_EDGE('',*,*,#8970,.T.);
#12067=ORIENTED_EDGE('',*,*,#8971,.T.);
#12068=ORIENTED_EDGE('',*,*,#8970,.F.);
#12069=ORIENTED_EDGE('',*,*,#8969,.T.);
#12070=ORIENTED_EDGE('',*,*,#8966,.T.);
#12071=ORIENTED_EDGE('',*,*,#8971,.F.);
#12072=ORIENTED_EDGE('',*,*,#8963,.T.);
#12073=ORIENTED_EDGE('',*,*,#8968,.F.);
#12074=CYLINDRICAL_SURFACE('',#14588,0.210000000000001);
#12075=CYLINDRICAL_SURFACE('',#14591,0.210000000000001);
#12076=CYLINDRICAL_SURFACE('',#14594,0.210000000000001);
#12077=CYLINDRICAL_SURFACE('',#14597,0.210000000000001);
#12078=CYLINDRICAL_SURFACE('',#14600,0.21);
#12079=CYLINDRICAL_SURFACE('',#14603,0.21);
#12080=CYLINDRICAL_SURFACE('',#14606,0.21);
#12081=CYLINDRICAL_SURFACE('',#14609,0.21);
#12082=CYLINDRICAL_SURFACE('',#14633,0.165);
#12083=CYLINDRICAL_SURFACE('',#14636,0.165);
#12084=CYLINDRICAL_SURFACE('',#14639,0.165);
#12085=CYLINDRICAL_SURFACE('',#14642,0.165);
#12086=CYLINDRICAL_SURFACE('',#14645,1.6);
#12087=CYLINDRICAL_SURFACE('',#14648,0.275);
#12088=CYLINDRICAL_SURFACE('',#14651,0.275);
#12089=CYLINDRICAL_SURFACE('',#14654,0.275);
#12090=CYLINDRICAL_SURFACE('',#14657,0.275);
#12091=CYLINDRICAL_SURFACE('',#14669,0.605);
#12092=CYLINDRICAL_SURFACE('',#14671,0.605);
#12093=CYLINDRICAL_SURFACE('',#14673,0.605);
#12094=CYLINDRICAL_SURFACE('',#14680,0.225);
#12095=CYLINDRICAL_SURFACE('',#14683,0.225);
#12096=CYLINDRICAL_SURFACE('',#14686,0.225);
#12097=CYLINDRICAL_SURFACE('',#14689,0.225);
#12098=CYLINDRICAL_SURFACE('',#14692,1.59);
#12099=CYLINDRICAL_SURFACE('',#14697,1.02);
#12100=CYLINDRICAL_SURFACE('',#14699,2.2);
#12101=CYLINDRICAL_SURFACE('',#14705,0.225);
#12102=CYLINDRICAL_SURFACE('',#14708,0.225);
#12103=CYLINDRICAL_SURFACE('',#14711,0.225);
#12104=CYLINDRICAL_SURFACE('',#14714,0.225);
#12105=CYLINDRICAL_SURFACE('',#14717,1.59);
#12106=CYLINDRICAL_SURFACE('',#14722,1.02);
#12107=CYLINDRICAL_SURFACE('',#14724,2.2);
#12108=CYLINDRICAL_SURFACE('',#14730,0.165);
#12109=CYLINDRICAL_SURFACE('',#14733,0.165);
#12110=CYLINDRICAL_SURFACE('',#14736,0.165);
#12111=CYLINDRICAL_SURFACE('',#14739,0.165);
#12112=CYLINDRICAL_SURFACE('',#14742,1.6);
#12113=CYLINDRICAL_SURFACE('',#14745,0.274999999999999);
#12114=CYLINDRICAL_SURFACE('',#14748,0.274999999999999);
#12115=CYLINDRICAL_SURFACE('',#14751,0.274999999999999);
#12116=CYLINDRICAL_SURFACE('',#14754,0.274999999999999);
#12117=CYLINDRICAL_SURFACE('',#14765,0.605);
#12118=CYLINDRICAL_SURFACE('',#14767,0.605);
#12119=CYLINDRICAL_SURFACE('',#14774,0.225);
#12120=CYLINDRICAL_SURFACE('',#14777,0.225);
#12121=CYLINDRICAL_SURFACE('',#14780,0.225);
#12122=CYLINDRICAL_SURFACE('',#14783,0.225);
#12123=CYLINDRICAL_SURFACE('',#14786,1.59);
#12124=CYLINDRICAL_SURFACE('',#14791,1.02);
#12125=CYLINDRICAL_SURFACE('',#14793,2.2);
#12126=CYLINDRICAL_SURFACE('',#14799,0.225);
#12127=CYLINDRICAL_SURFACE('',#14802,0.225);
#12128=CYLINDRICAL_SURFACE('',#14805,0.225);
#12129=CYLINDRICAL_SURFACE('',#14808,0.225);
#12130=CYLINDRICAL_SURFACE('',#14811,1.59);
#12131=CYLINDRICAL_SURFACE('',#14816,1.02);
#12132=CYLINDRICAL_SURFACE('',#14818,2.2);
#12133=CYLINDRICAL_SURFACE('',#14824,0.6);
#12134=CYLINDRICAL_SURFACE('',#14830,0.6);
#12135=CYLINDRICAL_SURFACE('',#14836,0.165);
#12136=CYLINDRICAL_SURFACE('',#14840,0.165);
#12137=CYLINDRICAL_SURFACE('',#14844,0.6);
#12138=CYLINDRICAL_SURFACE('',#14850,0.225);
#12139=CYLINDRICAL_SURFACE('',#14853,1.);
#12140=CYLINDRICAL_SURFACE('',#14859,0.225);
#12141=CYLINDRICAL_SURFACE('',#14862,1.);
#12142=CYLINDRICAL_SURFACE('',#14868,0.605);
#12143=CYLINDRICAL_SURFACE('',#14871,0.8);
#12144=CYLINDRICAL_SURFACE('',#14877,0.605);
#12145=CYLINDRICAL_SURFACE('',#14880,0.8);
#12146=CYLINDRICAL_SURFACE('',#14886,0.605);
#12147=CYLINDRICAL_SURFACE('',#14889,0.8);
#12148=CYLINDRICAL_SURFACE('',#14909,0.35);
#12149=CYLINDRICAL_SURFACE('',#14917,0.1954);
#12150=CYLINDRICAL_SURFACE('',#14920,0.274999999999999);
#12151=CYLINDRICAL_SURFACE('',#14923,0.274999999999999);
#12152=CYLINDRICAL_SURFACE('',#14926,0.274999999999999);
#12153=CYLINDRICAL_SURFACE('',#14929,0.274999999999999);
#12154=CYLINDRICAL_SURFACE('',#14932,0.275);
#12155=CYLINDRICAL_SURFACE('',#14935,0.275);
#12156=CYLINDRICAL_SURFACE('',#14938,0.275);
#12157=CYLINDRICAL_SURFACE('',#14941,0.275);
#12158=CYLINDRICAL_SURFACE('',#14951,0.21);
#12159=CYLINDRICAL_SURFACE('',#14954,0.21);
#12160=CYLINDRICAL_SURFACE('',#14957,0.21);
#12161=CYLINDRICAL_SURFACE('',#14960,0.21);
#12162=CYLINDRICAL_SURFACE('',#14973,0.605);
#12163=CYLINDRICAL_SURFACE('',#14975,0.605);
#12164=CYLINDRICAL_SURFACE('',#14977,0.605);
#12165=CYLINDRICAL_SURFACE('',#14984,0.210000000000001);
#12166=CYLINDRICAL_SURFACE('',#14987,0.210000000000001);
#12167=CYLINDRICAL_SURFACE('',#14990,0.210000000000001);
#12168=CYLINDRICAL_SURFACE('',#14993,0.210000000000001);
#12169=CYLINDRICAL_SURFACE('',#15004,0.605);
#12170=CYLINDRICAL_SURFACE('',#15006,0.605);
#12171=CYLINDRICAL_SURFACE('',#15013,0.6);
#12172=CYLINDRICAL_SURFACE('',#15019,0.6);
#12173=CYLINDRICAL_SURFACE('',#15025,0.165);
#12174=CYLINDRICAL_SURFACE('',#15029,0.165);
#12175=CYLINDRICAL_SURFACE('',#15033,0.6);
#12176=CYLINDRICAL_SURFACE('',#15039,0.225);
#12177=CYLINDRICAL_SURFACE('',#15042,1.);
#12178=CYLINDRICAL_SURFACE('',#15048,0.225);
#12179=CYLINDRICAL_SURFACE('',#15051,1.);
#12180=CYLINDRICAL_SURFACE('',#15057,0.605);
#12181=CYLINDRICAL_SURFACE('',#15060,0.8);
#12182=CYLINDRICAL_SURFACE('',#15066,0.605);
#12183=CYLINDRICAL_SURFACE('',#15069,0.8);
#12184=CYLINDRICAL_SURFACE('',#15075,0.605);
#12185=CYLINDRICAL_SURFACE('',#15078,0.8);
#12186=CYLINDRICAL_SURFACE('',#15084,0.605);
#12187=CYLINDRICAL_SURFACE('',#15087,0.8);
#12188=CYLINDRICAL_SURFACE('',#15097,0.425);
#12189=CYLINDRICAL_SURFACE('',#15105,0.24505);
#12190=CYLINDRICAL_SURFACE('',#15120,0.5);
#12191=CYLINDRICAL_SURFACE('',#15123,1.05);
#12192=CYLINDRICAL_SURFACE('',#15126,1.05);
#12193=CYLINDRICAL_SURFACE('',#15136,1.04);
#12194=CYLINDRICAL_SURFACE('',#15141,1.04);
#12195=CYLINDRICAL_SURFACE('',#15146,0.65);
#12196=CYLINDRICAL_SURFACE('',#15149,0.8);
#12197=CYLINDRICAL_SURFACE('',#15151,0.8);
#12198=CYLINDRICAL_SURFACE('',#15160,1.04);
#12199=CYLINDRICAL_SURFACE('',#15165,1.04);
#12200=CYLINDRICAL_SURFACE('',#15170,0.65);
#12201=CYLINDRICAL_SURFACE('',#15173,0.8);
#12202=CYLINDRICAL_SURFACE('',#15175,0.8);
#12203=CYLINDRICAL_SURFACE('',#15186,0.165);
#12204=CYLINDRICAL_SURFACE('',#15191,0.604999999999997);
#12205=CYLINDRICAL_SURFACE('',#15201,0.164999999999999);
#12206=CYLINDRICAL_SURFACE('',#15205,0.164999999999999);
#12207=CYLINDRICAL_SURFACE('',#15209,0.600000000000001);
#12208=CYLINDRICAL_SURFACE('',#15215,0.225000000000001);
#12209=CYLINDRICAL_SURFACE('',#15218,1.);
#12210=CYLINDRICAL_SURFACE('',#15224,0.225000000000001);
#12211=CYLINDRICAL_SURFACE('',#15227,1.);
#12212=CYLINDRICAL_SURFACE('',#15233,0.604999999999997);
#12213=CYLINDRICAL_SURFACE('',#15236,0.799999999999997);
#12214=CYLINDRICAL_SURFACE('',#15242,0.604999999999997);
#12215=CYLINDRICAL_SURFACE('',#15245,0.799999999999997);
#12216=CYLINDRICAL_SURFACE('',#15251,0.604999999999997);
#12217=CYLINDRICAL_SURFACE('',#15254,0.799999999999997);
#12218=CYLINDRICAL_SURFACE('',#15260,0.604999999999997);
#12219=CYLINDRICAL_SURFACE('',#15263,0.799999999999997);
#12220=CYLINDRICAL_SURFACE('',#15270,0.65);
#12221=CYLINDRICAL_SURFACE('',#15273,1.05);
#12222=CYLINDRICAL_SURFACE('',#15276,1.05);
#12223=CYLINDRICAL_SURFACE('',#15286,1.04);
#12224=CYLINDRICAL_SURFACE('',#15291,1.04);
#12225=CYLINDRICAL_SURFACE('',#15296,0.65);
#12226=CYLINDRICAL_SURFACE('',#15299,0.800000000000001);
#12227=CYLINDRICAL_SURFACE('',#15301,0.800000000000001);
#12228=CYLINDRICAL_SURFACE('',#15310,1.04);
#12229=CYLINDRICAL_SURFACE('',#15315,1.04);
#12230=CYLINDRICAL_SURFACE('',#15320,0.65);
#12231=CYLINDRICAL_SURFACE('',#15323,0.800000000000001);
#12232=CYLINDRICAL_SURFACE('',#15325,0.800000000000001);
#12233=CYLINDRICAL_SURFACE('',#15336,0.164999999999999);
#12234=CYLINDRICAL_SURFACE('',#15341,0.604999999999997);
#12235=CYLINDRICAL_SURFACE('',#15351,0.164999999999999);
#12236=CYLINDRICAL_SURFACE('',#15355,0.164999999999999);
#12237=CYLINDRICAL_SURFACE('',#15359,0.600000000000001);
#12238=CYLINDRICAL_SURFACE('',#15365,0.225000000000001);
#12239=CYLINDRICAL_SURFACE('',#15368,1.);
#12240=CYLINDRICAL_SURFACE('',#15374,0.225000000000001);
#12241=CYLINDRICAL_SURFACE('',#15377,1.);
#12242=CYLINDRICAL_SURFACE('',#15383,0.604999999999997);
#12243=CYLINDRICAL_SURFACE('',#15386,0.799999999999997);
#12244=CYLINDRICAL_SURFACE('',#15392,0.604999999999997);
#12245=CYLINDRICAL_SURFACE('',#15395,0.799999999999997);
#12246=CYLINDRICAL_SURFACE('',#15401,0.604999999999997);
#12247=CYLINDRICAL_SURFACE('',#15404,0.799999999999997);
#12248=CYLINDRICAL_SURFACE('',#15410,0.604999999999997);
#12249=CYLINDRICAL_SURFACE('',#15413,0.799999999999997);
#12250=CYLINDRICAL_SURFACE('',#15430,1.05);
#12251=CYLINDRICAL_SURFACE('',#15434,1.);
#12252=CYLINDRICAL_SURFACE('',#15438,1.05);
#12253=CYLINDRICAL_SURFACE('',#15442,1.);
#12254=CYLINDRICAL_SURFACE('',#15446,1.05);
#12255=CYLINDRICAL_SURFACE('',#15450,0.9);
#12256=CYLINDRICAL_SURFACE('',#15463,0.895);
#12257=CYLINDRICAL_SURFACE('',#15467,0.605);
#12258=CYLINDRICAL_SURFACE('',#15484,0.1954);
#12259=CYLINDRICAL_SURFACE('',#15487,1.);
#12260=CYLINDRICAL_SURFACE('',#15490,1.5);
#12261=CYLINDRICAL_SURFACE('',#15493,1.5);
#12262=CYLINDRICAL_SURFACE('',#15499,1.);
#12263=CYLINDRICAL_SURFACE('',#15502,1.5);
#12264=CYLINDRICAL_SURFACE('',#15509,1.);
#12265=CYLINDRICAL_SURFACE('',#15511,1.5);
#12266=CYLINDRICAL_SURFACE('',#15515,0.605);
#12267=CYLINDRICAL_SURFACE('',#15518,1.);
#12268=CYLINDRICAL_SURFACE('',#15524,0.604999999999997);
#12269=CYLINDRICAL_SURFACE('',#15527,1.);
#12270=CYLINDRICAL_SURFACE('',#15533,0.605);
#12271=CYLINDRICAL_SURFACE('',#15536,1.);
#12272=CYLINDRICAL_SURFACE('',#15542,1.);
#12273=CYLINDRICAL_SURFACE('',#15545,1.5);
#12274=CYLINDRICAL_SURFACE('',#15548,1.5);
#12275=CYLINDRICAL_SURFACE('',#15554,1.);
#12276=CYLINDRICAL_SURFACE('',#15557,1.5);
#12277=CYLINDRICAL_SURFACE('',#15564,1.);
#12278=CYLINDRICAL_SURFACE('',#15566,1.5);
#12279=CYLINDRICAL_SURFACE('',#15570,0.605);
#12280=CYLINDRICAL_SURFACE('',#15573,1.);
#12281=CYLINDRICAL_SURFACE('',#15579,0.604999999999997);
#12282=CYLINDRICAL_SURFACE('',#15582,1.);
#12283=CYLINDRICAL_SURFACE('',#15588,0.605);
#12284=CYLINDRICAL_SURFACE('',#15591,1.);
#12285=CYLINDRICAL_SURFACE('',#15597,0.164999999999999);
#12286=CYLINDRICAL_SURFACE('',#15601,0.164999999999999);
#12287=CYLINDRICAL_SURFACE('',#15605,0.600000000000001);
#12288=CYLINDRICAL_SURFACE('',#15611,0.225000000000001);
#12289=CYLINDRICAL_SURFACE('',#15614,1.);
#12290=CYLINDRICAL_SURFACE('',#15620,0.225000000000001);
#12291=CYLINDRICAL_SURFACE('',#15623,1.);
#12292=CYLINDRICAL_SURFACE('',#15629,0.605);
#12293=CYLINDRICAL_SURFACE('',#15632,0.800000000000001);
#12294=CYLINDRICAL_SURFACE('',#15638,0.605);
#12295=CYLINDRICAL_SURFACE('',#15641,0.800000000000001);
#12296=CYLINDRICAL_SURFACE('',#15647,0.605);
#12297=CYLINDRICAL_SURFACE('',#15650,0.800000000000001);
#12298=CYLINDRICAL_SURFACE('',#15656,0.605);
#12299=CYLINDRICAL_SURFACE('',#15659,0.800000000000001);
#12300=CYLINDRICAL_SURFACE('',#15665,0.605);
#12301=CYLINDRICAL_SURFACE('',#15668,0.800000000000001);
#12302=CYLINDRICAL_SURFACE('',#15678,0.35);
#12303=CYLINDRICAL_SURFACE('',#15686,0.1954);
#12304=CYLINDRICAL_SURFACE('',#15773,0.164999999999999);
#12305=CYLINDRICAL_SURFACE('',#15776,0.164999999999999);
#12306=CYLINDRICAL_SURFACE('',#15779,0.164999999999999);
#12307=CYLINDRICAL_SURFACE('',#15782,0.164999999999999);
#12308=CYLINDRICAL_SURFACE('',#15785,1.6);
#12309=CYLINDRICAL_SURFACE('',#15788,2.2);
#12310=CYLINDRICAL_SURFACE('',#15791,2.2);
#12311=CYLINDRICAL_SURFACE('',#15801,1.);
#12312=CYLINDRICAL_SURFACE('',#15803,1.5);
#12313=CYLINDRICAL_SURFACE('',#15806,1.);
#12314=CYLINDRICAL_SURFACE('',#15808,1.5);
#12315=CYLINDRICAL_SURFACE('',#15813,0.604999999999997);
#12316=CYLINDRICAL_SURFACE('',#15816,1.);
#12317=CYLINDRICAL_SURFACE('',#15822,0.605);
#12318=CYLINDRICAL_SURFACE('',#15825,1.);
#12319=CYLINDRICAL_SURFACE('',#15831,0.225000000000001);
#12320=CYLINDRICAL_SURFACE('',#15834,0.225000000000001);
#12321=CYLINDRICAL_SURFACE('',#15837,0.225000000000001);
#12322=CYLINDRICAL_SURFACE('',#15840,0.225000000000001);
#12323=CYLINDRICAL_SURFACE('',#15843,1.02);
#12324=CYLINDRICAL_SURFACE('',#15846,2.2);
#12325=CYLINDRICAL_SURFACE('',#15855,0.350000000000001);
#12326=CYLINDRICAL_SURFACE('',#15858,0.199999999999999);
#12327=CYLINDRICAL_SURFACE('',#15865,0.350000000000001);
#12328=CYLINDRICAL_SURFACE('',#15868,0.199999999999999);
#12329=CYLINDRICAL_SURFACE('',#15875,0.350000000000001);
#12330=CYLINDRICAL_SURFACE('',#15878,0.199999999999999);
#12331=CYLINDRICAL_SURFACE('',#15885,0.350000000000001);
#12332=CYLINDRICAL_SURFACE('',#15888,0.199999999999999);
#12333=CYLINDRICAL_SURFACE('',#15892,0.225000000000001);
#12334=CYLINDRICAL_SURFACE('',#15895,0.225000000000001);
#12335=CYLINDRICAL_SURFACE('',#15898,0.225000000000001);
#12336=CYLINDRICAL_SURFACE('',#15901,0.225000000000001);
#12337=CYLINDRICAL_SURFACE('',#15904,1.02);
#12338=CYLINDRICAL_SURFACE('',#15907,2.2);
#12339=CYLINDRICAL_SURFACE('',#15916,0.350000000000001);
#12340=CYLINDRICAL_SURFACE('',#15919,0.199999999999999);
#12341=CYLINDRICAL_SURFACE('',#15926,0.350000000000001);
#12342=CYLINDRICAL_SURFACE('',#15929,0.199999999999999);
#12343=CYLINDRICAL_SURFACE('',#15936,0.350000000000001);
#12344=CYLINDRICAL_SURFACE('',#15939,0.199999999999999);
#12345=CYLINDRICAL_SURFACE('',#15946,0.350000000000001);
#12346=CYLINDRICAL_SURFACE('',#15949,0.199999999999999);
#12347=CYLINDRICAL_SURFACE('',#15953,0.164999999999999);
#12348=CYLINDRICAL_SURFACE('',#15956,0.164999999999999);
#12349=CYLINDRICAL_SURFACE('',#15959,0.164999999999999);
#12350=CYLINDRICAL_SURFACE('',#15962,0.164999999999999);
#12351=CYLINDRICAL_SURFACE('',#15965,1.6);
#12352=CYLINDRICAL_SURFACE('',#15968,2.2);
#12353=CYLINDRICAL_SURFACE('',#15971,2.2);
#12354=CYLINDRICAL_SURFACE('',#15981,1.);
#12355=CYLINDRICAL_SURFACE('',#15983,1.5);
#12356=CYLINDRICAL_SURFACE('',#15986,1.);
#12357=CYLINDRICAL_SURFACE('',#15988,1.5);
#12358=CYLINDRICAL_SURFACE('',#15993,0.604999999999997);
#12359=CYLINDRICAL_SURFACE('',#15996,1.);
#12360=CYLINDRICAL_SURFACE('',#16002,0.605);
#12361=CYLINDRICAL_SURFACE('',#16005,1.);
#12362=CYLINDRICAL_SURFACE('',#16011,0.225000000000001);
#12363=CYLINDRICAL_SURFACE('',#16014,0.225000000000001);
#12364=CYLINDRICAL_SURFACE('',#16017,0.225000000000001);
#12365=CYLINDRICAL_SURFACE('',#16020,0.225000000000001);
#12366=CYLINDRICAL_SURFACE('',#16023,1.02);
#12367=CYLINDRICAL_SURFACE('',#16026,2.2);
#12368=CYLINDRICAL_SURFACE('',#16035,0.350000000000001);
#12369=CYLINDRICAL_SURFACE('',#16038,0.199999999999999);
#12370=CYLINDRICAL_SURFACE('',#16045,0.350000000000001);
#12371=CYLINDRICAL_SURFACE('',#16048,0.199999999999999);
#12372=CYLINDRICAL_SURFACE('',#16055,0.350000000000001);
#12373=CYLINDRICAL_SURFACE('',#16058,0.199999999999999);
#12374=CYLINDRICAL_SURFACE('',#16065,0.350000000000001);
#12375=CYLINDRICAL_SURFACE('',#16068,0.199999999999999);
#12376=CYLINDRICAL_SURFACE('',#16072,0.225000000000001);
#12377=CYLINDRICAL_SURFACE('',#16075,0.225000000000001);
#12378=CYLINDRICAL_SURFACE('',#16078,0.225000000000001);
#12379=CYLINDRICAL_SURFACE('',#16081,0.225000000000001);
#12380=CYLINDRICAL_SURFACE('',#16084,1.02);
#12381=CYLINDRICAL_SURFACE('',#16087,2.2);
#12382=CYLINDRICAL_SURFACE('',#16096,0.350000000000001);
#12383=CYLINDRICAL_SURFACE('',#16099,0.199999999999999);
#12384=CYLINDRICAL_SURFACE('',#16106,0.350000000000001);
#12385=CYLINDRICAL_SURFACE('',#16109,0.199999999999999);
#12386=CYLINDRICAL_SURFACE('',#16116,0.350000000000001);
#12387=CYLINDRICAL_SURFACE('',#16119,0.199999999999999);
#12388=CYLINDRICAL_SURFACE('',#16126,0.350000000000001);
#12389=CYLINDRICAL_SURFACE('',#16129,0.199999999999999);
#12390=CYLINDRICAL_SURFACE('',#16140,1.070235);
#12391=CYLINDRICAL_SURFACE('',#16142,0.6);
#12392=CYLINDRICAL_SURFACE('',#16148,1.070235);
#12393=CYLINDRICAL_SURFACE('',#16160,1.129765);
#12394=CYLINDRICAL_SURFACE('',#16167,1.6);
#12395=CYLINDRICAL_SURFACE('',#16172,1.129765);
#12396=CYLINDRICAL_SURFACE('',#16196,1.308355);
#12397=CYLINDRICAL_SURFACE('',#16201,0.891645);
#12398=CYLINDRICAL_SURFACE('',#16210,1.308355);
#12399=CYLINDRICAL_SURFACE('',#16212,0.891645);
#12400=CYLINDRICAL_SURFACE('',#16220,1.308355);
#12401=CYLINDRICAL_SURFACE('',#16229,0.891645);
#12402=CYLINDRICAL_SURFACE('',#16234,1.308355);
#12403=CYLINDRICAL_SURFACE('',#16240,0.891645);
#12404=CYLINDRICAL_SURFACE('',#16248,0.891645);
#12405=CYLINDRICAL_SURFACE('',#16257,1.308355);
#12406=CYLINDRICAL_SURFACE('',#16262,0.891645);
#12407=CYLINDRICAL_SURFACE('',#16268,1.308355);
#12408=CYLINDRICAL_SURFACE('',#16273,1.308355);
#12409=CYLINDRICAL_SURFACE('',#16285,0.891645);
#12410=CYLINDRICAL_SURFACE('',#16291,1.119765);
#12411=CYLINDRICAL_SURFACE('',#16295,1.085235);
#12412=CYLINDRICAL_SURFACE('',#16299,1.119765);
#12413=CYLINDRICAL_SURFACE('',#16303,1.085235);
#12414=CYLINDRICAL_SURFACE('',#16390,0.8);
#12415=CYLINDRICAL_SURFACE('',#16391,0.6);
#12416=CYLINDRICAL_SURFACE('',#16398,0.8);
#12417=CYLINDRICAL_SURFACE('',#16399,0.6);
#12418=CYLINDRICAL_SURFACE('',#16401,0.6);
#12419=CYLINDRICAL_SURFACE('',#16406,0.605);
#12420=CYLINDRICAL_SURFACE('',#16409,0.8);
#12421=CYLINDRICAL_SURFACE('',#16415,0.605);
#12422=CYLINDRICAL_SURFACE('',#16418,0.8);
#12423=CYLINDRICAL_SURFACE('',#16424,0.6);
#12424=CYLINDRICAL_SURFACE('',#16427,0.9);
#12425=CYLINDRICAL_SURFACE('',#16433,0.6);
#12426=CYLINDRICAL_SURFACE('',#16436,0.9);
#12427=CYLINDRICAL_SURFACE('',#16442,0.4);
#12428=CYLINDRICAL_SURFACE('',#16446,0.6);
#12429=CYLINDRICAL_SURFACE('',#16449,2.);
#12430=ADVANCED_FACE('',(#2063),#12074,.F.);
#12431=ADVANCED_FACE('',(#2064),#12075,.F.);
#12432=ADVANCED_FACE('',(#2065),#12076,.F.);
#12433=ADVANCED_FACE('',(#2066),#12077,.F.);
#12434=ADVANCED_FACE('',(#2067),#12078,.F.);
#12435=ADVANCED_FACE('',(#2068),#12079,.F.);
#12436=ADVANCED_FACE('',(#2069),#12080,.F.);
#12437=ADVANCED_FACE('',(#2070),#12081,.F.);
#12438=ADVANCED_FACE('',(#2071),#1640,.T.);
#12439=ADVANCED_FACE('',(#2072),#1641,.T.);
#12440=ADVANCED_FACE('',(#2073),#1642,.T.);
#12441=ADVANCED_FACE('',(#2074),#1643,.T.);
#12442=ADVANCED_FACE('',(#2075,#1215,#1216,#1217,#1218,#1219,#1220,#1221,
#1222),#1644,.T.);
#12443=ADVANCED_FACE('',(#2076,#1223,#1224,#1225,#1226,#1227,#1228,#1229,
#1230),#1645,.F.);
#12444=ADVANCED_FACE('',(#2077),#1646,.T.);
#12445=ADVANCED_FACE('',(#2078),#1647,.T.);
#12446=ADVANCED_FACE('',(#2079),#1648,.T.);
#12447=ADVANCED_FACE('',(#2080),#1649,.T.);
#12448=ADVANCED_FACE('',(#2081),#1650,.T.);
#12449=ADVANCED_FACE('',(#2082),#1651,.F.);
#12450=ADVANCED_FACE('',(#2083),#1652,.T.);
#12451=ADVANCED_FACE('',(#2084),#1653,.T.);
#12452=ADVANCED_FACE('',(#2085),#1654,.T.);
#12453=ADVANCED_FACE('',(#2086),#1655,.T.);
#12454=ADVANCED_FACE('',(#2087),#1656,.T.);
#12455=ADVANCED_FACE('',(#2088),#1657,.F.);
#12456=ADVANCED_FACE('',(#2089),#12082,.F.);
#12457=ADVANCED_FACE('',(#2090),#12083,.F.);
#12458=ADVANCED_FACE('',(#2091),#12084,.F.);
#12459=ADVANCED_FACE('',(#2092),#12085,.F.);
#12460=ADVANCED_FACE('',(#2093),#12086,.F.);
#12461=ADVANCED_FACE('',(#2094),#12087,.F.);
#12462=ADVANCED_FACE('',(#2095),#12088,.F.);
#12463=ADVANCED_FACE('',(#2096),#12089,.F.);
#12464=ADVANCED_FACE('',(#2097),#12090,.F.);
#12465=ADVANCED_FACE('',(#2098,#1231,#1232),#1658,.T.);
#12466=ADVANCED_FACE('',(#2099,#1233,#1234),#1659,.T.);
#12467=ADVANCED_FACE('',(#2100),#1660,.T.);
#12468=ADVANCED_FACE('',(#2101),#1661,.T.);
#12469=ADVANCED_FACE('',(#2102,#1235),#1662,.T.);
#12470=ADVANCED_FACE('',(#2103,#1236,#1237,#1238,#1239,#1240,#1241,#1242),
#1663,.T.);
#12471=ADVANCED_FACE('',(#2104),#12091,.F.);
#12472=ADVANCED_FACE('',(#2105),#12092,.F.);
#12473=ADVANCED_FACE('',(#2106),#12093,.F.);
#12474=ADVANCED_FACE('',(#2107,#1243,#1244,#1245,#1246,#1247,#1248,#1249),
#1664,.T.);
#12475=ADVANCED_FACE('',(#2108,#1250),#1665,.T.);
#12476=ADVANCED_FACE('',(#2109),#1666,.T.);
#12477=ADVANCED_FACE('',(#2110,#1251,#1252,#1253,#1254),#1667,.F.);
#12478=ADVANCED_FACE('',(#2111),#12094,.F.);
#12479=ADVANCED_FACE('',(#2112),#12095,.F.);
#12480=ADVANCED_FACE('',(#2113),#12096,.F.);
#12481=ADVANCED_FACE('',(#2114),#12097,.F.);
#12482=ADVANCED_FACE('',(#2115),#12098,.T.);
#12483=ADVANCED_FACE('',(#2116,#1255),#1668,.T.);
#12484=ADVANCED_FACE('',(#2117),#12099,.F.);
#12485=ADVANCED_FACE('',(#2118),#12100,.T.);
#12486=ADVANCED_FACE('',(#2119,#1256,#1257,#1258,#1259,#1260),#1669,.T.);
#12487=ADVANCED_FACE('',(#2120,#1261,#1262,#1263,#1264,#1265),#1670,.F.);
#12488=ADVANCED_FACE('',(#2121),#12101,.F.);
#12489=ADVANCED_FACE('',(#2122),#12102,.F.);
#12490=ADVANCED_FACE('',(#2123),#12103,.F.);
#12491=ADVANCED_FACE('',(#2124),#12104,.F.);
#12492=ADVANCED_FACE('',(#2125),#12105,.T.);
#12493=ADVANCED_FACE('',(#2126,#1266),#1671,.F.);
#12494=ADVANCED_FACE('',(#2127),#12106,.F.);
#12495=ADVANCED_FACE('',(#2128),#12107,.T.);
#12496=ADVANCED_FACE('',(#2129,#1267,#1268,#1269,#1270,#1271),#1672,.T.);
#12497=ADVANCED_FACE('',(#2130,#1272,#1273,#1274,#1275,#1276),#1673,.F.);
#12498=ADVANCED_FACE('',(#2131),#12108,.F.);
#12499=ADVANCED_FACE('',(#2132),#12109,.F.);
#12500=ADVANCED_FACE('',(#2133),#12110,.F.);
#12501=ADVANCED_FACE('',(#2134),#12111,.F.);
#12502=ADVANCED_FACE('',(#2135),#12112,.F.);
#12503=ADVANCED_FACE('',(#2136),#12113,.F.);
#12504=ADVANCED_FACE('',(#2137),#12114,.F.);
#12505=ADVANCED_FACE('',(#2138),#12115,.F.);
#12506=ADVANCED_FACE('',(#2139),#12116,.F.);
#12507=ADVANCED_FACE('',(#2140,#1277,#1278),#1674,.T.);
#12508=ADVANCED_FACE('',(#2141,#1279,#1280),#1675,.T.);
#12509=ADVANCED_FACE('',(#2142),#1676,.T.);
#12510=ADVANCED_FACE('',(#2143),#1677,.T.);
#12511=ADVANCED_FACE('',(#2144),#1678,.T.);
#12512=ADVANCED_FACE('',(#2145,#1281,#1282,#1283,#1284,#1285,#1286,#1287),
#1679,.T.);
#12513=ADVANCED_FACE('',(#2146),#12117,.F.);
#12514=ADVANCED_FACE('',(#2147),#12118,.F.);
#12515=ADVANCED_FACE('',(#2148,#1288,#1289,#1290,#1291,#1292,#1293,#1294),
#1680,.T.);
#12516=ADVANCED_FACE('',(#2149),#1681,.T.);
#12517=ADVANCED_FACE('',(#2150),#1682,.T.);
#12518=ADVANCED_FACE('',(#2151,#1295,#1296,#1297,#1298),#1683,.F.);
#12519=ADVANCED_FACE('',(#2152),#12119,.F.);
#12520=ADVANCED_FACE('',(#2153),#12120,.F.);
#12521=ADVANCED_FACE('',(#2154),#12121,.F.);
#12522=ADVANCED_FACE('',(#2155),#12122,.F.);
#12523=ADVANCED_FACE('',(#2156),#12123,.T.);
#12524=ADVANCED_FACE('',(#2157,#1299),#1684,.T.);
#12525=ADVANCED_FACE('',(#2158),#12124,.F.);
#12526=ADVANCED_FACE('',(#2159),#12125,.T.);
#12527=ADVANCED_FACE('',(#2160,#1300,#1301,#1302,#1303,#1304),#1685,.T.);
#12528=ADVANCED_FACE('',(#2161,#1305,#1306,#1307,#1308,#1309),#1686,.F.);
#12529=ADVANCED_FACE('',(#2162),#12126,.F.);
#12530=ADVANCED_FACE('',(#2163),#12127,.F.);
#12531=ADVANCED_FACE('',(#2164),#12128,.F.);
#12532=ADVANCED_FACE('',(#2165),#12129,.F.);
#12533=ADVANCED_FACE('',(#2166),#12130,.T.);
#12534=ADVANCED_FACE('',(#2167,#1310),#1687,.F.);
#12535=ADVANCED_FACE('',(#2168),#12131,.F.);
#12536=ADVANCED_FACE('',(#2169),#12132,.T.);
#12537=ADVANCED_FACE('',(#2170,#1311,#1312,#1313,#1314,#1315),#1688,.T.);
#12538=ADVANCED_FACE('',(#2171,#1316,#1317,#1318,#1319,#1320),#1689,.F.);
#12539=ADVANCED_FACE('',(#2172),#12133,.T.);
#12540=ADVANCED_FACE('',(#2173),#1690,.T.);
#12541=ADVANCED_FACE('',(#2174),#1691,.F.);
#12542=ADVANCED_FACE('',(#2175),#12134,.T.);
#12543=ADVANCED_FACE('',(#2176),#1692,.T.);
#12544=ADVANCED_FACE('',(#2177),#1693,.F.);
#12545=ADVANCED_FACE('',(#2178),#12135,.F.);
#12546=ADVANCED_FACE('',(#2179),#1694,.T.);
#12547=ADVANCED_FACE('',(#2180),#12136,.F.);
#12548=ADVANCED_FACE('',(#2181),#1695,.F.);
#12549=ADVANCED_FACE('',(#2182),#12137,.T.);
#12550=ADVANCED_FACE('',(#2183,#1321),#1696,.T.);
#12551=ADVANCED_FACE('',(#2184,#1322),#1697,.F.);
#12552=ADVANCED_FACE('',(#2185),#12138,.F.);
#12553=ADVANCED_FACE('',(#2186),#12139,.T.);
#12554=ADVANCED_FACE('',(#2187,#1323),#1698,.T.);
#12555=ADVANCED_FACE('',(#2188,#1324),#1699,.F.);
#12556=ADVANCED_FACE('',(#2189),#12140,.F.);
#12557=ADVANCED_FACE('',(#2190),#12141,.T.);
#12558=ADVANCED_FACE('',(#2191,#1325),#1700,.T.);
#12559=ADVANCED_FACE('',(#2192,#1326),#1701,.F.);
#12560=ADVANCED_FACE('',(#2193),#12142,.F.);
#12561=ADVANCED_FACE('',(#2194),#12143,.T.);
#12562=ADVANCED_FACE('',(#2195,#1327),#1702,.T.);
#12563=ADVANCED_FACE('',(#2196,#1328),#1703,.F.);
#12564=ADVANCED_FACE('',(#2197),#12144,.F.);
#12565=ADVANCED_FACE('',(#2198),#12145,.T.);
#12566=ADVANCED_FACE('',(#2199,#1329),#1704,.T.);
#12567=ADVANCED_FACE('',(#2200,#1330),#1705,.F.);
#12568=ADVANCED_FACE('',(#2201),#12146,.F.);
#12569=ADVANCED_FACE('',(#2202),#12147,.T.);
#12570=ADVANCED_FACE('',(#2203,#1331),#1706,.T.);
#12571=ADVANCED_FACE('',(#2204,#1332),#1707,.F.);
#12572=ADVANCED_FACE('',(#2205),#1708,.F.);
#12573=ADVANCED_FACE('',(#2206),#1709,.F.);
#12574=ADVANCED_FACE('',(#2207),#1710,.F.);
#12575=ADVANCED_FACE('',(#2208),#1711,.F.);
#12576=ADVANCED_FACE('',(#2209),#1712,.F.);
#12577=ADVANCED_FACE('',(#2210),#1713,.F.);
#12578=ADVANCED_FACE('',(#2211),#1714,.F.);
#12579=ADVANCED_FACE('',(#2212),#1715,.F.);
#12580=ADVANCED_FACE('',(#2213),#1716,.F.);
#12581=ADVANCED_FACE('',(#2214),#1717,.T.);
#12582=ADVANCED_FACE('',(#2215),#729,.T.);
#12583=ADVANCED_FACE('',(#2216),#12148,.T.);
#12584=ADVANCED_FACE('',(#2217),#730,.T.);
#12585=ADVANCED_FACE('',(#2218,#1333),#1718,.T.);
#12586=ADVANCED_FACE('',(#2219),#731,.T.);
#12587=ADVANCED_FACE('',(#2220),#12149,.T.);
#12588=ADVANCED_FACE('',(#2221),#12150,.F.);
#12589=ADVANCED_FACE('',(#2222),#12151,.F.);
#12590=ADVANCED_FACE('',(#2223),#12152,.F.);
#12591=ADVANCED_FACE('',(#2224),#12153,.F.);
#12592=ADVANCED_FACE('',(#2225),#12154,.F.);
#12593=ADVANCED_FACE('',(#2226),#12155,.F.);
#12594=ADVANCED_FACE('',(#2227),#12156,.F.);
#12595=ADVANCED_FACE('',(#2228),#12157,.F.);
#12596=ADVANCED_FACE('',(#2229),#1719,.T.);
#12597=ADVANCED_FACE('',(#2230),#1720,.T.);
#12598=ADVANCED_FACE('',(#2231),#1721,.T.);
#12599=ADVANCED_FACE('',(#2232),#1722,.T.);
#12600=ADVANCED_FACE('',(#2233,#1334,#1335,#1336,#1337,#1338,#1339,#1340,
#1341),#1723,.T.);
#12601=ADVANCED_FACE('',(#2234,#1342,#1343,#1344,#1345,#1346,#1347,#1348,
#1349),#1724,.F.);
#12602=ADVANCED_FACE('',(#2235),#12158,.F.);
#12603=ADVANCED_FACE('',(#2236),#12159,.F.);
#12604=ADVANCED_FACE('',(#2237),#12160,.F.);
#12605=ADVANCED_FACE('',(#2238),#12161,.F.);
#12606=ADVANCED_FACE('',(#2239,#1350,#1351,#1352,#1353,#1354),#1725,.F.);
#12607=ADVANCED_FACE('',(#2240),#1726,.T.);
#12608=ADVANCED_FACE('',(#2241),#1727,.T.);
#12609=ADVANCED_FACE('',(#2242),#1728,.T.);
#12610=ADVANCED_FACE('',(#2243),#1729,.T.);
#12611=ADVANCED_FACE('',(#2244,#1355),#1730,.T.);
#12612=ADVANCED_FACE('',(#2245,#1356,#1357),#1731,.T.);
#12613=ADVANCED_FACE('',(#2246),#12162,.F.);
#12614=ADVANCED_FACE('',(#2247),#12163,.F.);
#12615=ADVANCED_FACE('',(#2248),#12164,.F.);
#12616=ADVANCED_FACE('',(#2249,#1358),#1732,.T.);
#12617=ADVANCED_FACE('',(#2250,#1359,#1360),#1733,.T.);
#12618=ADVANCED_FACE('',(#2251,#1361,#1362,#1363,#1364),#1734,.T.);
#12619=ADVANCED_FACE('',(#2252),#1735,.F.);
#12620=ADVANCED_FACE('',(#2253),#12165,.F.);
#12621=ADVANCED_FACE('',(#2254),#12166,.F.);
#12622=ADVANCED_FACE('',(#2255),#12167,.F.);
#12623=ADVANCED_FACE('',(#2256),#12168,.F.);
#12624=ADVANCED_FACE('',(#2257,#1365,#1366),#1736,.F.);
#12625=ADVANCED_FACE('',(#2258),#1737,.T.);
#12626=ADVANCED_FACE('',(#2259),#1738,.T.);
#12627=ADVANCED_FACE('',(#2260,#1367,#1368),#1739,.F.);
#12628=ADVANCED_FACE('',(#2261,#1369,#1370),#1740,.T.);
#12629=ADVANCED_FACE('',(#2262),#1741,.T.);
#12630=ADVANCED_FACE('',(#2263),#12169,.F.);
#12631=ADVANCED_FACE('',(#2264),#12170,.F.);
#12632=ADVANCED_FACE('',(#2265),#1742,.T.);
#12633=ADVANCED_FACE('',(#2266,#1371,#1372),#1743,.T.);
#12634=ADVANCED_FACE('',(#2267,#1373,#1374,#1375,#1376),#1744,.T.);
#12635=ADVANCED_FACE('',(#2268),#1745,.F.);
#12636=ADVANCED_FACE('',(#2269),#12171,.T.);
#12637=ADVANCED_FACE('',(#2270),#1746,.T.);
#12638=ADVANCED_FACE('',(#2271),#1747,.F.);
#12639=ADVANCED_FACE('',(#2272),#12172,.T.);
#12640=ADVANCED_FACE('',(#2273),#1748,.T.);
#12641=ADVANCED_FACE('',(#2274),#1749,.F.);
#12642=ADVANCED_FACE('',(#2275),#12173,.F.);
#12643=ADVANCED_FACE('',(#2276),#1750,.T.);
#12644=ADVANCED_FACE('',(#2277),#12174,.F.);
#12645=ADVANCED_FACE('',(#2278),#1751,.F.);
#12646=ADVANCED_FACE('',(#2279),#12175,.T.);
#12647=ADVANCED_FACE('',(#2280,#1377),#1752,.T.);
#12648=ADVANCED_FACE('',(#2281,#1378),#1753,.F.);
#12649=ADVANCED_FACE('',(#2282),#12176,.F.);
#12650=ADVANCED_FACE('',(#2283),#12177,.T.);
#12651=ADVANCED_FACE('',(#2284,#1379),#1754,.T.);
#12652=ADVANCED_FACE('',(#2285,#1380),#1755,.F.);
#12653=ADVANCED_FACE('',(#2286),#12178,.F.);
#12654=ADVANCED_FACE('',(#2287),#12179,.T.);
#12655=ADVANCED_FACE('',(#2288,#1381),#1756,.T.);
#12656=ADVANCED_FACE('',(#2289,#1382),#1757,.F.);
#12657=ADVANCED_FACE('',(#2290),#12180,.F.);
#12658=ADVANCED_FACE('',(#2291),#12181,.T.);
#12659=ADVANCED_FACE('',(#2292,#1383),#1758,.T.);
#12660=ADVANCED_FACE('',(#2293,#1384),#1759,.F.);
#12661=ADVANCED_FACE('',(#2294),#12182,.F.);
#12662=ADVANCED_FACE('',(#2295),#12183,.T.);
#12663=ADVANCED_FACE('',(#2296,#1385),#1760,.T.);
#12664=ADVANCED_FACE('',(#2297,#1386),#1761,.F.);
#12665=ADVANCED_FACE('',(#2298),#12184,.F.);
#12666=ADVANCED_FACE('',(#2299),#12185,.T.);
#12667=ADVANCED_FACE('',(#2300,#1387),#1762,.T.);
#12668=ADVANCED_FACE('',(#2301,#1388),#1763,.F.);
#12669=ADVANCED_FACE('',(#2302),#12186,.F.);
#12670=ADVANCED_FACE('',(#2303),#12187,.T.);
#12671=ADVANCED_FACE('',(#2304,#1389),#1764,.T.);
#12672=ADVANCED_FACE('',(#2305,#1390),#1765,.F.);
#12673=ADVANCED_FACE('',(#2306),#1766,.T.);
#12674=ADVANCED_FACE('',(#2307),#732,.T.);
#12675=ADVANCED_FACE('',(#2308),#12188,.T.);
#12676=ADVANCED_FACE('',(#2309),#733,.T.);
#12677=ADVANCED_FACE('',(#2310,#1391),#1767,.T.);
#12678=ADVANCED_FACE('',(#2311),#734,.T.);
#12679=ADVANCED_FACE('',(#2312),#12189,.T.);
#12680=ADVANCED_FACE('',(#2313),#735,.T.);
#12681=ADVANCED_FACE('',(#2314),#1768,.T.);
#12682=ADVANCED_FACE('',(#2315),#1769,.F.);
#12683=ADVANCED_FACE('',(#2316),#1770,.F.);
#12684=ADVANCED_FACE('',(#2317),#1771,.F.);
#12685=ADVANCED_FACE('',(#2318),#1772,.F.);
#12686=ADVANCED_FACE('',(#2319),#1773,.F.);
#12687=ADVANCED_FACE('',(#2320),#1774,.F.);
#12688=ADVANCED_FACE('',(#2321),#1775,.F.);
#12689=ADVANCED_FACE('',(#2322),#1776,.F.);
#12690=ADVANCED_FACE('',(#2323),#12190,.F.);
#12691=ADVANCED_FACE('',(#2324),#12191,.F.);
#12692=ADVANCED_FACE('',(#2325),#12192,.F.);
#12693=ADVANCED_FACE('',(#2326),#1777,.T.);
#12694=ADVANCED_FACE('',(#2327,#1392,#1393,#1394),#1778,.T.);
#12695=ADVANCED_FACE('',(#2328),#1779,.T.);
#12696=ADVANCED_FACE('',(#2329,#1395,#1396,#1397),#1780,.T.);
#12697=ADVANCED_FACE('',(#2330),#1781,.T.);
#12698=ADVANCED_FACE('',(#2331),#1782,.F.);
#12699=ADVANCED_FACE('',(#2332),#12193,.T.);
#12700=ADVANCED_FACE('',(#2333,#1398),#1783,.T.);
#12701=ADVANCED_FACE('',(#2334),#12194,.T.);
#12702=ADVANCED_FACE('',(#2335,#1399),#1784,.T.);
#12703=ADVANCED_FACE('',(#2336),#12195,.F.);
#12704=ADVANCED_FACE('',(#2337),#12196,.F.);
#12705=ADVANCED_FACE('',(#2338),#12197,.F.);
#12706=ADVANCED_FACE('',(#2339),#1785,.T.);
#12707=ADVANCED_FACE('',(#2340),#1786,.T.);
#12708=ADVANCED_FACE('',(#2341),#1787,.T.);
#12709=ADVANCED_FACE('',(#2342),#1788,.T.);
#12710=ADVANCED_FACE('',(#2343,#1400,#1401,#1402),#1789,.T.);
#12711=ADVANCED_FACE('',(#2344,#1403,#1404,#1405),#1790,.F.);
#12712=ADVANCED_FACE('',(#2345),#12198,.T.);
#12713=ADVANCED_FACE('',(#2346,#1406),#1791,.F.);
#12714=ADVANCED_FACE('',(#2347),#12199,.T.);
#12715=ADVANCED_FACE('',(#2348,#1407),#1792,.F.);
#12716=ADVANCED_FACE('',(#2349),#12200,.F.);
#12717=ADVANCED_FACE('',(#2350),#12201,.F.);
#12718=ADVANCED_FACE('',(#2351),#12202,.F.);
#12719=ADVANCED_FACE('',(#2352),#1793,.T.);
#12720=ADVANCED_FACE('',(#2353),#1794,.T.);
#12721=ADVANCED_FACE('',(#2354),#1795,.T.);
#12722=ADVANCED_FACE('',(#2355),#1796,.T.);
#12723=ADVANCED_FACE('',(#2356,#1408,#1409,#1410),#1797,.T.);
#12724=ADVANCED_FACE('',(#2357,#1411,#1412,#1413),#1798,.F.);
#12725=ADVANCED_FACE('',(#2358),#1799,.T.);
#12726=ADVANCED_FACE('',(#2359),#12203,.F.);
#12727=ADVANCED_FACE('',(#2360),#1800,.T.);
#12728=ADVANCED_FACE('',(#2361,#1414),#12204,.F.);
#12729=ADVANCED_FACE('',(#2362,#1415),#1801,.T.);
#12730=ADVANCED_FACE('',(#2363,#1416),#1802,.T.);
#12731=ADVANCED_FACE('',(#2364,#1417),#1803,.T.);
#12732=ADVANCED_FACE('',(#2365),#1804,.T.);
#12733=ADVANCED_FACE('',(#2366),#1805,.T.);
#12734=ADVANCED_FACE('',(#2367),#1806,.F.);
#12735=ADVANCED_FACE('',(#2368),#12205,.F.);
#12736=ADVANCED_FACE('',(#2369),#1807,.T.);
#12737=ADVANCED_FACE('',(#2370),#12206,.F.);
#12738=ADVANCED_FACE('',(#2371),#1808,.F.);
#12739=ADVANCED_FACE('',(#2372),#12207,.T.);
#12740=ADVANCED_FACE('',(#2373,#1418),#1809,.T.);
#12741=ADVANCED_FACE('',(#2374,#1419),#1810,.F.);
#12742=ADVANCED_FACE('',(#2375),#12208,.F.);
#12743=ADVANCED_FACE('',(#2376),#12209,.T.);
#12744=ADVANCED_FACE('',(#2377,#1420),#1811,.T.);
#12745=ADVANCED_FACE('',(#2378,#1421),#1812,.F.);
#12746=ADVANCED_FACE('',(#2379),#12210,.F.);
#12747=ADVANCED_FACE('',(#2380),#12211,.T.);
#12748=ADVANCED_FACE('',(#2381,#1422),#1813,.T.);
#12749=ADVANCED_FACE('',(#2382,#1423),#1814,.F.);
#12750=ADVANCED_FACE('',(#2383),#12212,.F.);
#12751=ADVANCED_FACE('',(#2384),#12213,.T.);
#12752=ADVANCED_FACE('',(#2385,#1424),#1815,.T.);
#12753=ADVANCED_FACE('',(#2386,#1425),#1816,.F.);
#12754=ADVANCED_FACE('',(#2387),#12214,.F.);
#12755=ADVANCED_FACE('',(#2388),#12215,.T.);
#12756=ADVANCED_FACE('',(#2389,#1426),#1817,.T.);
#12757=ADVANCED_FACE('',(#2390,#1427),#1818,.F.);
#12758=ADVANCED_FACE('',(#2391),#12216,.F.);
#12759=ADVANCED_FACE('',(#2392),#12217,.T.);
#12760=ADVANCED_FACE('',(#2393,#1428),#1819,.T.);
#12761=ADVANCED_FACE('',(#2394,#1429),#1820,.F.);
#12762=ADVANCED_FACE('',(#2395),#12218,.F.);
#12763=ADVANCED_FACE('',(#2396),#12219,.T.);
#12764=ADVANCED_FACE('',(#2397,#1430),#1821,.T.);
#12765=ADVANCED_FACE('',(#2398,#1431),#1822,.F.);
#12766=ADVANCED_FACE('',(#2399),#12220,.F.);
#12767=ADVANCED_FACE('',(#2400),#12221,.F.);
#12768=ADVANCED_FACE('',(#2401),#12222,.F.);
#12769=ADVANCED_FACE('',(#2402),#1823,.T.);
#12770=ADVANCED_FACE('',(#2403,#1432,#1433,#1434),#1824,.T.);
#12771=ADVANCED_FACE('',(#2404),#1825,.T.);
#12772=ADVANCED_FACE('',(#2405,#1435,#1436,#1437),#1826,.T.);
#12773=ADVANCED_FACE('',(#2406),#1827,.T.);
#12774=ADVANCED_FACE('',(#2407),#1828,.F.);
#12775=ADVANCED_FACE('',(#2408),#12223,.T.);
#12776=ADVANCED_FACE('',(#2409,#1438),#1829,.T.);
#12777=ADVANCED_FACE('',(#2410),#12224,.T.);
#12778=ADVANCED_FACE('',(#2411,#1439),#1830,.T.);
#12779=ADVANCED_FACE('',(#2412),#12225,.F.);
#12780=ADVANCED_FACE('',(#2413),#12226,.F.);
#12781=ADVANCED_FACE('',(#2414),#12227,.F.);
#12782=ADVANCED_FACE('',(#2415),#1831,.T.);
#12783=ADVANCED_FACE('',(#2416),#1832,.T.);
#12784=ADVANCED_FACE('',(#2417),#1833,.T.);
#12785=ADVANCED_FACE('',(#2418),#1834,.T.);
#12786=ADVANCED_FACE('',(#2419,#1440,#1441,#1442),#1835,.T.);
#12787=ADVANCED_FACE('',(#2420,#1443,#1444,#1445),#1836,.F.);
#12788=ADVANCED_FACE('',(#2421),#12228,.T.);
#12789=ADVANCED_FACE('',(#2422,#1446),#1837,.F.);
#12790=ADVANCED_FACE('',(#2423),#12229,.T.);
#12791=ADVANCED_FACE('',(#2424,#1447),#1838,.F.);
#12792=ADVANCED_FACE('',(#2425),#12230,.F.);
#12793=ADVANCED_FACE('',(#2426),#12231,.F.);
#12794=ADVANCED_FACE('',(#2427),#12232,.F.);
#12795=ADVANCED_FACE('',(#2428),#1839,.T.);
#12796=ADVANCED_FACE('',(#2429),#1840,.T.);
#12797=ADVANCED_FACE('',(#2430),#1841,.T.);
#12798=ADVANCED_FACE('',(#2431),#1842,.T.);
#12799=ADVANCED_FACE('',(#2432,#1448,#1449,#1450),#1843,.T.);
#12800=ADVANCED_FACE('',(#2433,#1451,#1452,#1453),#1844,.F.);
#12801=ADVANCED_FACE('',(#2434),#1845,.T.);
#12802=ADVANCED_FACE('',(#2435),#12233,.F.);
#12803=ADVANCED_FACE('',(#2436),#1846,.T.);
#12804=ADVANCED_FACE('',(#2437,#1454),#12234,.F.);
#12805=ADVANCED_FACE('',(#2438,#1455),#1847,.T.);
#12806=ADVANCED_FACE('',(#2439,#1456),#1848,.T.);
#12807=ADVANCED_FACE('',(#2440,#1457),#1849,.T.);
#12808=ADVANCED_FACE('',(#2441),#1850,.T.);
#12809=ADVANCED_FACE('',(#2442),#1851,.T.);
#12810=ADVANCED_FACE('',(#2443),#1852,.F.);
#12811=ADVANCED_FACE('',(#2444),#12235,.F.);
#12812=ADVANCED_FACE('',(#2445),#1853,.T.);
#12813=ADVANCED_FACE('',(#2446),#12236,.F.);
#12814=ADVANCED_FACE('',(#2447),#1854,.F.);
#12815=ADVANCED_FACE('',(#2448),#12237,.T.);
#12816=ADVANCED_FACE('',(#2449,#1458),#1855,.T.);
#12817=ADVANCED_FACE('',(#2450,#1459),#1856,.F.);
#12818=ADVANCED_FACE('',(#2451),#12238,.F.);
#12819=ADVANCED_FACE('',(#2452),#12239,.T.);
#12820=ADVANCED_FACE('',(#2453,#1460),#1857,.T.);
#12821=ADVANCED_FACE('',(#2454,#1461),#1858,.F.);
#12822=ADVANCED_FACE('',(#2455),#12240,.F.);
#12823=ADVANCED_FACE('',(#2456),#12241,.T.);
#12824=ADVANCED_FACE('',(#2457,#1462),#1859,.T.);
#12825=ADVANCED_FACE('',(#2458,#1463),#1860,.F.);
#12826=ADVANCED_FACE('',(#2459),#12242,.F.);
#12827=ADVANCED_FACE('',(#2460),#12243,.T.);
#12828=ADVANCED_FACE('',(#2461,#1464),#1861,.T.);
#12829=ADVANCED_FACE('',(#2462,#1465),#1862,.F.);
#12830=ADVANCED_FACE('',(#2463),#12244,.F.);
#12831=ADVANCED_FACE('',(#2464),#12245,.T.);
#12832=ADVANCED_FACE('',(#2465,#1466),#1863,.T.);
#12833=ADVANCED_FACE('',(#2466,#1467),#1864,.F.);
#12834=ADVANCED_FACE('',(#2467),#12246,.F.);
#12835=ADVANCED_FACE('',(#2468),#12247,.T.);
#12836=ADVANCED_FACE('',(#2469,#1468),#1865,.T.);
#12837=ADVANCED_FACE('',(#2470,#1469),#1866,.F.);
#12838=ADVANCED_FACE('',(#2471),#12248,.F.);
#12839=ADVANCED_FACE('',(#2472),#12249,.T.);
#12840=ADVANCED_FACE('',(#2473,#1470),#1867,.T.);
#12841=ADVANCED_FACE('',(#2474,#1471),#1868,.F.);
#12842=ADVANCED_FACE('',(#2475),#1869,.F.);
#12843=ADVANCED_FACE('',(#2476),#1870,.F.);
#12844=ADVANCED_FACE('',(#2477),#1871,.F.);
#12845=ADVANCED_FACE('',(#2478),#1872,.F.);
#12846=ADVANCED_FACE('',(#2479),#1873,.F.);
#12847=ADVANCED_FACE('',(#2480,#1472),#1874,.T.);
#12848=ADVANCED_FACE('',(#2481),#12250,.T.);
#12849=ADVANCED_FACE('',(#2482,#1473),#1875,.T.);
#12850=ADVANCED_FACE('',(#2483),#12251,.T.);
#12851=ADVANCED_FACE('',(#2484,#1474),#1876,.T.);
#12852=ADVANCED_FACE('',(#2485),#12252,.T.);
#12853=ADVANCED_FACE('',(#2486,#1475),#1877,.T.);
#12854=ADVANCED_FACE('',(#2487),#12253,.T.);
#12855=ADVANCED_FACE('',(#2488,#1476),#1878,.T.);
#12856=ADVANCED_FACE('',(#2489),#12254,.T.);
#12857=ADVANCED_FACE('',(#2490,#1477),#1879,.T.);
#12858=ADVANCED_FACE('',(#2491,#1478),#12255,.F.);
#12859=ADVANCED_FACE('',(#2492),#1880,.F.);
#12860=ADVANCED_FACE('',(#2493),#1881,.F.);
#12861=ADVANCED_FACE('',(#2494),#1882,.F.);
#12862=ADVANCED_FACE('',(#2495),#1883,.F.);
#12863=ADVANCED_FACE('',(#2496,#1479),#1884,.T.);
#12864=ADVANCED_FACE('',(#2497,#1480),#12256,.T.);
#12865=ADVANCED_FACE('',(#2498,#1481),#1885,.T.);
#12866=ADVANCED_FACE('',(#2499,#1482),#12257,.F.);
#12867=ADVANCED_FACE('',(#2500),#1886,.F.);
#12868=ADVANCED_FACE('',(#2501),#1887,.F.);
#12869=ADVANCED_FACE('',(#2502),#1888,.F.);
#12870=ADVANCED_FACE('',(#2503),#1889,.F.);
#12871=ADVANCED_FACE('',(#2504),#1890,.F.);
#12872=ADVANCED_FACE('',(#2505),#1891,.F.);
#12873=ADVANCED_FACE('',(#2506),#1892,.F.);
#12874=ADVANCED_FACE('',(#2507),#1893,.F.);
#12875=ADVANCED_FACE('',(#2508,#1483),#1894,.T.);
#12876=ADVANCED_FACE('',(#2509),#736,.T.);
#12877=ADVANCED_FACE('',(#2510),#12258,.T.);
#12878=ADVANCED_FACE('',(#2511),#12259,.F.);
#12879=ADVANCED_FACE('',(#2512),#12260,.T.);
#12880=ADVANCED_FACE('',(#2513),#12261,.T.);
#12881=ADVANCED_FACE('',(#2514),#1895,.T.);
#12882=ADVANCED_FACE('',(#2515),#1896,.T.);
#12883=ADVANCED_FACE('',(#2516),#1897,.T.);
#12884=ADVANCED_FACE('',(#2517),#12262,.F.);
#12885=ADVANCED_FACE('',(#2518),#12263,.T.);
#12886=ADVANCED_FACE('',(#2519,#1484,#1485,#1486),#1898,.F.);
#12887=ADVANCED_FACE('',(#2520),#1899,.T.);
#12888=ADVANCED_FACE('',(#2521),#12264,.F.);
#12889=ADVANCED_FACE('',(#2522),#12265,.T.);
#12890=ADVANCED_FACE('',(#2523,#1487,#1488,#1489),#1900,.T.);
#12891=ADVANCED_FACE('',(#2524),#12266,.F.);
#12892=ADVANCED_FACE('',(#2525),#12267,.T.);
#12893=ADVANCED_FACE('',(#2526,#1490),#1901,.T.);
#12894=ADVANCED_FACE('',(#2527,#1491),#1902,.F.);
#12895=ADVANCED_FACE('',(#2528),#12268,.F.);
#12896=ADVANCED_FACE('',(#2529),#12269,.T.);
#12897=ADVANCED_FACE('',(#2530,#1492),#1903,.T.);
#12898=ADVANCED_FACE('',(#2531,#1493),#1904,.F.);
#12899=ADVANCED_FACE('',(#2532),#12270,.F.);
#12900=ADVANCED_FACE('',(#2533),#12271,.T.);
#12901=ADVANCED_FACE('',(#2534,#1494),#1905,.T.);
#12902=ADVANCED_FACE('',(#2535,#1495),#1906,.F.);
#12903=ADVANCED_FACE('',(#2536),#12272,.F.);
#12904=ADVANCED_FACE('',(#2537),#12273,.T.);
#12905=ADVANCED_FACE('',(#2538),#12274,.T.);
#12906=ADVANCED_FACE('',(#2539),#1907,.T.);
#12907=ADVANCED_FACE('',(#2540),#1908,.T.);
#12908=ADVANCED_FACE('',(#2541),#1909,.T.);
#12909=ADVANCED_FACE('',(#2542),#12275,.F.);
#12910=ADVANCED_FACE('',(#2543),#12276,.T.);
#12911=ADVANCED_FACE('',(#2544,#1496,#1497,#1498),#1910,.F.);
#12912=ADVANCED_FACE('',(#2545),#1911,.T.);
#12913=ADVANCED_FACE('',(#2546),#12277,.F.);
#12914=ADVANCED_FACE('',(#2547),#12278,.T.);
#12915=ADVANCED_FACE('',(#2548,#1499,#1500,#1501),#1912,.T.);
#12916=ADVANCED_FACE('',(#2549),#12279,.F.);
#12917=ADVANCED_FACE('',(#2550),#12280,.T.);
#12918=ADVANCED_FACE('',(#2551,#1502),#1913,.T.);
#12919=ADVANCED_FACE('',(#2552,#1503),#1914,.F.);
#12920=ADVANCED_FACE('',(#2553),#12281,.F.);
#12921=ADVANCED_FACE('',(#2554),#12282,.T.);
#12922=ADVANCED_FACE('',(#2555,#1504),#1915,.T.);
#12923=ADVANCED_FACE('',(#2556,#1505),#1916,.F.);
#12924=ADVANCED_FACE('',(#2557),#12283,.F.);
#12925=ADVANCED_FACE('',(#2558),#12284,.T.);
#12926=ADVANCED_FACE('',(#2559,#1506),#1917,.T.);
#12927=ADVANCED_FACE('',(#2560,#1507),#1918,.F.);
#12928=ADVANCED_FACE('',(#2561),#12285,.F.);
#12929=ADVANCED_FACE('',(#2562),#1919,.T.);
#12930=ADVANCED_FACE('',(#2563),#12286,.F.);
#12931=ADVANCED_FACE('',(#2564),#1920,.F.);
#12932=ADVANCED_FACE('',(#2565),#12287,.T.);
#12933=ADVANCED_FACE('',(#2566,#1508),#1921,.T.);
#12934=ADVANCED_FACE('',(#2567,#1509),#1922,.F.);
#12935=ADVANCED_FACE('',(#2568),#12288,.F.);
#12936=ADVANCED_FACE('',(#2569),#12289,.T.);
#12937=ADVANCED_FACE('',(#2570,#1510),#1923,.T.);
#12938=ADVANCED_FACE('',(#2571,#1511),#1924,.F.);
#12939=ADVANCED_FACE('',(#2572),#12290,.F.);
#12940=ADVANCED_FACE('',(#2573),#12291,.T.);
#12941=ADVANCED_FACE('',(#2574,#1512),#1925,.T.);
#12942=ADVANCED_FACE('',(#2575,#1513),#1926,.F.);
#12943=ADVANCED_FACE('',(#2576),#12292,.F.);
#12944=ADVANCED_FACE('',(#2577),#12293,.T.);
#12945=ADVANCED_FACE('',(#2578,#1514),#1927,.T.);
#12946=ADVANCED_FACE('',(#2579,#1515),#1928,.F.);
#12947=ADVANCED_FACE('',(#2580),#12294,.F.);
#12948=ADVANCED_FACE('',(#2581),#12295,.T.);
#12949=ADVANCED_FACE('',(#2582,#1516),#1929,.T.);
#12950=ADVANCED_FACE('',(#2583,#1517),#1930,.F.);
#12951=ADVANCED_FACE('',(#2584),#12296,.F.);
#12952=ADVANCED_FACE('',(#2585),#12297,.T.);
#12953=ADVANCED_FACE('',(#2586,#1518),#1931,.T.);
#12954=ADVANCED_FACE('',(#2587,#1519),#1932,.F.);
#12955=ADVANCED_FACE('',(#2588),#12298,.F.);
#12956=ADVANCED_FACE('',(#2589),#12299,.T.);
#12957=ADVANCED_FACE('',(#2590,#1520),#1933,.T.);
#12958=ADVANCED_FACE('',(#2591,#1521),#1934,.F.);
#12959=ADVANCED_FACE('',(#2592),#12300,.F.);
#12960=ADVANCED_FACE('',(#2593),#12301,.T.);
#12961=ADVANCED_FACE('',(#2594,#1522),#1935,.T.);
#12962=ADVANCED_FACE('',(#2595,#1523),#1936,.F.);
#12963=ADVANCED_FACE('',(#2596),#1937,.T.);
#12964=ADVANCED_FACE('',(#2597),#737,.T.);
#12965=ADVANCED_FACE('',(#2598),#12302,.T.);
#12966=ADVANCED_FACE('',(#2599),#738,.T.);
#12967=ADVANCED_FACE('',(#2600,#1524),#1938,.T.);
#12968=ADVANCED_FACE('',(#2601),#739,.T.);
#12969=ADVANCED_FACE('',(#2602),#12303,.T.);
#12970=ADVANCED_FACE('',(#2603),#740,.T.);
#12971=ADVANCED_FACE('',(#2604),#1939,.T.);
#12972=ADVANCED_FACE('',(#2605),#1940,.F.);
#12973=ADVANCED_FACE('',(#2606),#1941,.F.);
#12974=ADVANCED_FACE('',(#2607),#1942,.F.);
#12975=ADVANCED_FACE('',(#2608),#1943,.F.);
#12976=ADVANCED_FACE('',(#2609),#1944,.F.);
#12977=ADVANCED_FACE('',(#2610),#1945,.F.);
#12978=ADVANCED_FACE('',(#2611),#1946,.F.);
#12979=ADVANCED_FACE('',(#2612),#1947,.F.);
#12980=ADVANCED_FACE('',(#2613),#12304,.F.);
#12981=ADVANCED_FACE('',(#2614),#12305,.F.);
#12982=ADVANCED_FACE('',(#2615),#12306,.F.);
#12983=ADVANCED_FACE('',(#2616),#12307,.F.);
#12984=ADVANCED_FACE('',(#2617),#12308,.F.);
#12985=ADVANCED_FACE('',(#2618),#12309,.T.);
#12986=ADVANCED_FACE('',(#2619),#12310,.T.);
#12987=ADVANCED_FACE('',(#2620),#1948,.T.);
#12988=ADVANCED_FACE('',(#2621,#1525,#1526,#1527,#1528,#1529,#1530,#1531),
#1949,.T.);
#12989=ADVANCED_FACE('',(#2622),#1950,.T.);
#12990=ADVANCED_FACE('',(#2623),#12311,.F.);
#12991=ADVANCED_FACE('',(#2624),#12312,.T.);
#12992=ADVANCED_FACE('',(#2625),#1951,.T.);
#12993=ADVANCED_FACE('',(#2626),#12313,.F.);
#12994=ADVANCED_FACE('',(#2627),#12314,.T.);
#12995=ADVANCED_FACE('',(#2628),#1952,.T.);
#12996=ADVANCED_FACE('',(#2629,#1532,#1533,#1534,#1535,#1536,#1537,#1538),
#1953,.F.);
#12997=ADVANCED_FACE('',(#2630),#12315,.F.);
#12998=ADVANCED_FACE('',(#2631),#12316,.T.);
#12999=ADVANCED_FACE('',(#2632,#1539),#1954,.T.);
#13000=ADVANCED_FACE('',(#2633,#1540),#1955,.F.);
#13001=ADVANCED_FACE('',(#2634),#12317,.F.);
#13002=ADVANCED_FACE('',(#2635),#12318,.T.);
#13003=ADVANCED_FACE('',(#2636,#1541),#1956,.T.);
#13004=ADVANCED_FACE('',(#2637,#1542),#1957,.F.);
#13005=ADVANCED_FACE('',(#2638),#12319,.F.);
#13006=ADVANCED_FACE('',(#2639),#12320,.F.);
#13007=ADVANCED_FACE('',(#2640),#12321,.F.);
#13008=ADVANCED_FACE('',(#2641),#12322,.F.);
#13009=ADVANCED_FACE('',(#2642),#12323,.F.);
#13010=ADVANCED_FACE('',(#2643),#12324,.T.);
#13011=ADVANCED_FACE('',(#2644,#1543,#1544,#1545,#1546,#1547),#1958,.T.);
#13012=ADVANCED_FACE('',(#2645,#1548,#1549,#1550,#1551,#1552),#1959,.F.);
#13013=ADVANCED_FACE('',(#2646,#1553),#1960,.T.);
#13014=ADVANCED_FACE('',(#2647),#12325,.T.);
#13015=ADVANCED_FACE('',(#2648),#1961,.F.);
#13016=ADVANCED_FACE('',(#2649),#12326,.T.);
#13017=ADVANCED_FACE('',(#2650),#1962,.T.);
#13018=ADVANCED_FACE('',(#2651,#1554),#1963,.T.);
#13019=ADVANCED_FACE('',(#2652),#12327,.T.);
#13020=ADVANCED_FACE('',(#2653),#1964,.F.);
#13021=ADVANCED_FACE('',(#2654),#12328,.T.);
#13022=ADVANCED_FACE('',(#2655),#1965,.T.);
#13023=ADVANCED_FACE('',(#2656,#1555),#1966,.T.);
#13024=ADVANCED_FACE('',(#2657),#12329,.T.);
#13025=ADVANCED_FACE('',(#2658),#1967,.F.);
#13026=ADVANCED_FACE('',(#2659),#12330,.T.);
#13027=ADVANCED_FACE('',(#2660),#1968,.T.);
#13028=ADVANCED_FACE('',(#2661,#1556),#1969,.T.);
#13029=ADVANCED_FACE('',(#2662),#12331,.T.);
#13030=ADVANCED_FACE('',(#2663),#1970,.F.);
#13031=ADVANCED_FACE('',(#2664),#12332,.T.);
#13032=ADVANCED_FACE('',(#2665),#1971,.T.);
#13033=ADVANCED_FACE('',(#2666),#12333,.F.);
#13034=ADVANCED_FACE('',(#2667),#12334,.F.);
#13035=ADVANCED_FACE('',(#2668),#12335,.F.);
#13036=ADVANCED_FACE('',(#2669),#12336,.F.);
#13037=ADVANCED_FACE('',(#2670),#12337,.F.);
#13038=ADVANCED_FACE('',(#2671),#12338,.T.);
#13039=ADVANCED_FACE('',(#2672,#1557,#1558,#1559,#1560,#1561),#1972,.T.);
#13040=ADVANCED_FACE('',(#2673,#1562,#1563,#1564,#1565,#1566),#1973,.F.);
#13041=ADVANCED_FACE('',(#2674,#1567),#1974,.F.);
#13042=ADVANCED_FACE('',(#2675),#12339,.T.);
#13043=ADVANCED_FACE('',(#2676),#1975,.T.);
#13044=ADVANCED_FACE('',(#2677),#12340,.T.);
#13045=ADVANCED_FACE('',(#2678),#1976,.F.);
#13046=ADVANCED_FACE('',(#2679,#1568),#1977,.F.);
#13047=ADVANCED_FACE('',(#2680),#12341,.T.);
#13048=ADVANCED_FACE('',(#2681),#1978,.T.);
#13049=ADVANCED_FACE('',(#2682),#12342,.T.);
#13050=ADVANCED_FACE('',(#2683),#1979,.F.);
#13051=ADVANCED_FACE('',(#2684,#1569),#1980,.F.);
#13052=ADVANCED_FACE('',(#2685),#12343,.T.);
#13053=ADVANCED_FACE('',(#2686),#1981,.T.);
#13054=ADVANCED_FACE('',(#2687),#12344,.T.);
#13055=ADVANCED_FACE('',(#2688),#1982,.F.);
#13056=ADVANCED_FACE('',(#2689,#1570),#1983,.F.);
#13057=ADVANCED_FACE('',(#2690),#12345,.T.);
#13058=ADVANCED_FACE('',(#2691),#1984,.T.);
#13059=ADVANCED_FACE('',(#2692),#12346,.T.);
#13060=ADVANCED_FACE('',(#2693),#1985,.F.);
#13061=ADVANCED_FACE('',(#2694),#12347,.F.);
#13062=ADVANCED_FACE('',(#2695),#12348,.F.);
#13063=ADVANCED_FACE('',(#2696),#12349,.F.);
#13064=ADVANCED_FACE('',(#2697),#12350,.F.);
#13065=ADVANCED_FACE('',(#2698),#12351,.F.);
#13066=ADVANCED_FACE('',(#2699),#12352,.T.);
#13067=ADVANCED_FACE('',(#2700),#12353,.T.);
#13068=ADVANCED_FACE('',(#2701),#1986,.T.);
#13069=ADVANCED_FACE('',(#2702,#1571,#1572,#1573,#1574,#1575,#1576,#1577),
#1987,.T.);
#13070=ADVANCED_FACE('',(#2703),#1988,.T.);
#13071=ADVANCED_FACE('',(#2704),#12354,.F.);
#13072=ADVANCED_FACE('',(#2705),#12355,.T.);
#13073=ADVANCED_FACE('',(#2706),#1989,.T.);
#13074=ADVANCED_FACE('',(#2707),#12356,.F.);
#13075=ADVANCED_FACE('',(#2708),#12357,.T.);
#13076=ADVANCED_FACE('',(#2709),#1990,.T.);
#13077=ADVANCED_FACE('',(#2710,#1578,#1579,#1580,#1581,#1582,#1583,#1584),
#1991,.F.);
#13078=ADVANCED_FACE('',(#2711),#12358,.F.);
#13079=ADVANCED_FACE('',(#2712),#12359,.T.);
#13080=ADVANCED_FACE('',(#2713,#1585),#1992,.T.);
#13081=ADVANCED_FACE('',(#2714,#1586),#1993,.F.);
#13082=ADVANCED_FACE('',(#2715),#12360,.F.);
#13083=ADVANCED_FACE('',(#2716),#12361,.T.);
#13084=ADVANCED_FACE('',(#2717,#1587),#1994,.T.);
#13085=ADVANCED_FACE('',(#2718,#1588),#1995,.F.);
#13086=ADVANCED_FACE('',(#2719),#12362,.F.);
#13087=ADVANCED_FACE('',(#2720),#12363,.F.);
#13088=ADVANCED_FACE('',(#2721),#12364,.F.);
#13089=ADVANCED_FACE('',(#2722),#12365,.F.);
#13090=ADVANCED_FACE('',(#2723),#12366,.F.);
#13091=ADVANCED_FACE('',(#2724),#12367,.T.);
#13092=ADVANCED_FACE('',(#2725,#1589,#1590,#1591,#1592,#1593),#1996,.T.);
#13093=ADVANCED_FACE('',(#2726,#1594,#1595,#1596,#1597,#1598),#1997,.F.);
#13094=ADVANCED_FACE('',(#2727,#1599),#1998,.T.);
#13095=ADVANCED_FACE('',(#2728),#12368,.T.);
#13096=ADVANCED_FACE('',(#2729),#1999,.F.);
#13097=ADVANCED_FACE('',(#2730),#12369,.T.);
#13098=ADVANCED_FACE('',(#2731),#2000,.T.);
#13099=ADVANCED_FACE('',(#2732,#1600),#2001,.T.);
#13100=ADVANCED_FACE('',(#2733),#12370,.T.);
#13101=ADVANCED_FACE('',(#2734),#2002,.F.);
#13102=ADVANCED_FACE('',(#2735),#12371,.T.);
#13103=ADVANCED_FACE('',(#2736),#2003,.T.);
#13104=ADVANCED_FACE('',(#2737,#1601),#2004,.T.);
#13105=ADVANCED_FACE('',(#2738),#12372,.T.);
#13106=ADVANCED_FACE('',(#2739),#2005,.F.);
#13107=ADVANCED_FACE('',(#2740),#12373,.T.);
#13108=ADVANCED_FACE('',(#2741),#2006,.T.);
#13109=ADVANCED_FACE('',(#2742,#1602),#2007,.T.);
#13110=ADVANCED_FACE('',(#2743),#12374,.T.);
#13111=ADVANCED_FACE('',(#2744),#2008,.F.);
#13112=ADVANCED_FACE('',(#2745),#12375,.T.);
#13113=ADVANCED_FACE('',(#2746),#2009,.T.);
#13114=ADVANCED_FACE('',(#2747),#12376,.F.);
#13115=ADVANCED_FACE('',(#2748),#12377,.F.);
#13116=ADVANCED_FACE('',(#2749),#12378,.F.);
#13117=ADVANCED_FACE('',(#2750),#12379,.F.);
#13118=ADVANCED_FACE('',(#2751),#12380,.F.);
#13119=ADVANCED_FACE('',(#2752),#12381,.T.);
#13120=ADVANCED_FACE('',(#2753,#1603,#1604,#1605,#1606,#1607),#2010,.T.);
#13121=ADVANCED_FACE('',(#2754,#1608,#1609,#1610,#1611,#1612),#2011,.F.);
#13122=ADVANCED_FACE('',(#2755,#1613),#2012,.F.);
#13123=ADVANCED_FACE('',(#2756),#12382,.T.);
#13124=ADVANCED_FACE('',(#2757),#2013,.T.);
#13125=ADVANCED_FACE('',(#2758),#12383,.T.);
#13126=ADVANCED_FACE('',(#2759),#2014,.F.);
#13127=ADVANCED_FACE('',(#2760,#1614),#2015,.F.);
#13128=ADVANCED_FACE('',(#2761),#12384,.T.);
#13129=ADVANCED_FACE('',(#2762),#2016,.T.);
#13130=ADVANCED_FACE('',(#2763),#12385,.T.);
#13131=ADVANCED_FACE('',(#2764),#2017,.F.);
#13132=ADVANCED_FACE('',(#2765,#1615),#2018,.F.);
#13133=ADVANCED_FACE('',(#2766),#12386,.T.);
#13134=ADVANCED_FACE('',(#2767),#2019,.T.);
#13135=ADVANCED_FACE('',(#2768),#12387,.T.);
#13136=ADVANCED_FACE('',(#2769),#2020,.F.);
#13137=ADVANCED_FACE('',(#2770,#1616),#2021,.F.);
#13138=ADVANCED_FACE('',(#2771),#12388,.T.);
#13139=ADVANCED_FACE('',(#2772),#2022,.T.);
#13140=ADVANCED_FACE('',(#2773),#12389,.T.);
#13141=ADVANCED_FACE('',(#2774),#2023,.F.);
#13142=ADVANCED_FACE('',(#2775),#35,.F.);
#13143=ADVANCED_FACE('',(#2776),#12390,.T.);
#13144=ADVANCED_FACE('',(#2777),#12391,.F.);
#13145=ADVANCED_FACE('',(#2778),#741,.F.);
#13146=ADVANCED_FACE('',(#2779,#1617),#2024,.T.);
#13147=ADVANCED_FACE('',(#2780),#12392,.T.);
#13148=ADVANCED_FACE('',(#2781,#1618),#2025,.T.);
#13149=ADVANCED_FACE('',(#2782),#742,.F.);
#13150=ADVANCED_FACE('',(#2783),#36,.F.);
#13151=ADVANCED_FACE('',(#2784),#12393,.F.);
#13152=ADVANCED_FACE('',(#2785,#1619),#2026,.T.);
#13153=ADVANCED_FACE('',(#2786),#743,.T.);
#13154=ADVANCED_FACE('',(#2787),#12394,.T.);
#13155=ADVANCED_FACE('',(#2788),#744,.T.);
#13156=ADVANCED_FACE('',(#2789,#1620),#2027,.T.);
#13157=ADVANCED_FACE('',(#2790),#12395,.F.);
#13158=ADVANCED_FACE('',(#2791),#14,.T.);
#13159=ADVANCED_FACE('',(#2792),#15,.T.);
#13160=ADVANCED_FACE('',(#2793),#16,.T.);
#13161=ADVANCED_FACE('',(#2794),#17,.T.);
#13162=ADVANCED_FACE('',(#2795),#18,.T.);
#13163=ADVANCED_FACE('',(#2796),#19,.T.);
#13164=ADVANCED_FACE('',(#2797),#20,.T.);
#13165=ADVANCED_FACE('',(#2798),#21,.F.);
#13166=ADVANCED_FACE('',(#2799),#2028,.T.);
#13167=ADVANCED_FACE('',(#2800),#12396,.T.);
#13168=ADVANCED_FACE('',(#2801),#2029,.T.);
#13169=ADVANCED_FACE('',(#2802),#12397,.F.);
#13170=ADVANCED_FACE('',(#2803),#22,.F.);
#13171=ADVANCED_FACE('',(#2804),#23,.F.);
#13172=ADVANCED_FACE('',(#2805),#2030,.T.);
#13173=ADVANCED_FACE('',(#2806),#12398,.T.);
#13174=ADVANCED_FACE('',(#2807),#12399,.F.);
#13175=ADVANCED_FACE('',(#2808),#2031,.T.);
#13176=ADVANCED_FACE('',(#2809),#24,.F.);
#13177=ADVANCED_FACE('',(#2810),#25,.F.);
#13178=ADVANCED_FACE('',(#2811),#12400,.T.);
#13179=ADVANCED_FACE('',(#2812),#2032,.T.);
#13180=ADVANCED_FACE('',(#2813),#2033,.T.);
#13181=ADVANCED_FACE('',(#2814),#12401,.F.);
#13182=ADVANCED_FACE('',(#2815),#26,.F.);
#13183=ADVANCED_FACE('',(#2816),#27,.F.);
#13184=ADVANCED_FACE('',(#2817),#12402,.T.);
#13185=ADVANCED_FACE('',(#2818),#2034,.T.);
#13186=ADVANCED_FACE('',(#2819),#12403,.F.);
#13187=ADVANCED_FACE('',(#2820),#2035,.T.);
#13188=ADVANCED_FACE('',(#2821),#28,.F.);
#13189=ADVANCED_FACE('',(#2822),#29,.F.);
#13190=ADVANCED_FACE('',(#2823),#12404,.F.);
#13191=ADVANCED_FACE('',(#2824),#2036,.T.);
#13192=ADVANCED_FACE('',(#2825),#2037,.T.);
#13193=ADVANCED_FACE('',(#2826),#12405,.T.);
#13194=ADVANCED_FACE('',(#2827),#30,.F.);
#13195=ADVANCED_FACE('',(#2828),#31,.F.);
#13196=ADVANCED_FACE('',(#2829),#12406,.F.);
#13197=ADVANCED_FACE('',(#2830),#2038,.T.);
#13198=ADVANCED_FACE('',(#2831),#12407,.T.);
#13199=ADVANCED_FACE('',(#2832),#2039,.T.);
#13200=ADVANCED_FACE('',(#2833),#32,.F.);
#13201=ADVANCED_FACE('',(#2834),#12408,.T.);
#13202=ADVANCED_FACE('',(#2835),#2040,.T.);
#13203=ADVANCED_FACE('',(#2836),#33,.F.);
#13204=ADVANCED_FACE('',(#2837),#2041,.T.);
#13205=ADVANCED_FACE('',(#2838),#12409,.F.);
#13206=ADVANCED_FACE('',(#2839),#34,.F.);
#13207=ADVANCED_FACE('',(#2840,#1621),#2042,.T.);
#13208=ADVANCED_FACE('',(#2841),#12410,.T.);
#13209=ADVANCED_FACE('',(#2842,#1622),#2043,.T.);
#13210=ADVANCED_FACE('',(#2843),#12411,.F.);
#13211=ADVANCED_FACE('',(#2844,#1623),#2044,.T.);
#13212=ADVANCED_FACE('',(#2845),#12412,.T.);
#13213=ADVANCED_FACE('',(#2846,#1624),#2045,.T.);
#13214=ADVANCED_FACE('',(#2847),#12413,.F.);
#13215=ADVANCED_FACE('',(#2848,#1625),#2046,.T.);
#13216=ADVANCED_FACE('',(#2849,#1626),#2047,.F.);
#13217=ADVANCED_FACE('',(#2850),#12414,.T.);
#13218=ADVANCED_FACE('',(#2851),#12415,.T.);
#13219=ADVANCED_FACE('',(#2852,#1627),#2048,.T.);
#13220=ADVANCED_FACE('',(#2853,#1628),#2049,.F.);
#13221=ADVANCED_FACE('',(#2854),#12416,.T.);
#13222=ADVANCED_FACE('',(#2855),#12417,.T.);
#13223=ADVANCED_FACE('',(#2856),#12418,.T.);
#13224=ADVANCED_FACE('',(#2857),#2050,.T.);
#13225=ADVANCED_FACE('',(#2858),#2051,.F.);
#13226=ADVANCED_FACE('',(#2859),#12419,.F.);
#13227=ADVANCED_FACE('',(#2860),#12420,.T.);
#13228=ADVANCED_FACE('',(#2861,#1629),#2052,.T.);
#13229=ADVANCED_FACE('',(#2862,#1630),#2053,.F.);
#13230=ADVANCED_FACE('',(#2863),#12421,.F.);
#13231=ADVANCED_FACE('',(#2864),#12422,.T.);
#13232=ADVANCED_FACE('',(#2865,#1631),#2054,.T.);
#13233=ADVANCED_FACE('',(#2866,#1632),#2055,.F.);
#13234=ADVANCED_FACE('',(#2867),#12423,.F.);
#13235=ADVANCED_FACE('',(#2868),#12424,.T.);
#13236=ADVANCED_FACE('',(#2869,#1633),#2056,.T.);
#13237=ADVANCED_FACE('',(#2870,#1634),#2057,.F.);
#13238=ADVANCED_FACE('',(#2871),#12425,.F.);
#13239=ADVANCED_FACE('',(#2872),#12426,.T.);
#13240=ADVANCED_FACE('',(#2873,#1635),#2058,.T.);
#13241=ADVANCED_FACE('',(#2874,#1636),#2059,.F.);
#13242=ADVANCED_FACE('',(#2875),#12427,.T.);
#13243=ADVANCED_FACE('',(#2876),#2060,.F.);
#13244=ADVANCED_FACE('',(#2877),#12428,.F.);
#13245=ADVANCED_FACE('',(#2878),#12429,.T.);
#13246=ADVANCED_FACE('',(#2879,#1637),#2061,.T.);
#13247=ADVANCED_FACE('',(#2880,#1638,#1639),#2062,.F.);
#13248=CLOSED_SHELL('',(#12430,#12431,#12432,#12433,#12434,#12435,#12436,
#12437,#12438,#12439,#12440,#12441,#12442,#12443));
#13249=CLOSED_SHELL('',(#12444,#12445,#12446,#12447,#12448,#12449));
#13250=CLOSED_SHELL('',(#12450,#12451,#12452,#12453,#12454,#12455));
#13251=CLOSED_SHELL('',(#12456,#12457,#12458,#12459,#12460,#12461,#12462,
#12463,#12464,#12465,#12466,#12467,#12468,#12469,#12470,#12471,#12472,#12473,
#12474,#12475,#12476,#12477));
#13252=CLOSED_SHELL('',(#12478,#12479,#12480,#12481,#12482,#12483,#12484,
#12485,#12486,#12487));
#13253=CLOSED_SHELL('',(#12488,#12489,#12490,#12491,#12492,#12493,#12494,
#12495,#12496,#12497));
#13254=CLOSED_SHELL('',(#12498,#12499,#12500,#12501,#12502,#12503,#12504,
#12505,#12506,#12507,#12508,#12509,#12510,#12511,#12512,#12513,#12514,#12515,
#12516,#12517,#12518));
#13255=CLOSED_SHELL('',(#12519,#12520,#12521,#12522,#12523,#12524,#12525,
#12526,#12527,#12528));
#13256=CLOSED_SHELL('',(#12529,#12530,#12531,#12532,#12533,#12534,#12535,
#12536,#12537,#12538));
#13257=CLOSED_SHELL('',(#12539,#12540,#12541));
#13258=CLOSED_SHELL('',(#12542,#12543,#12544));
#13259=CLOSED_SHELL('',(#12545,#12546,#12547,#12548,#12549,#12550,#12551));
#13260=CLOSED_SHELL('',(#12552,#12553,#12554,#12555));
#13261=CLOSED_SHELL('',(#12556,#12557,#12558,#12559));
#13262=CLOSED_SHELL('',(#12560,#12561,#12562,#12563));
#13263=CLOSED_SHELL('',(#12564,#12565,#12566,#12567));
#13264=CLOSED_SHELL('',(#12568,#12569,#12570,#12571));
#13265=CLOSED_SHELL('',(#12572,#12573,#12574,#12575,#12576,#12577,#12578,
#12579));
#13266=CLOSED_SHELL('',(#12580,#12581,#12582,#12583,#12584,#12585,#12586,
#12587));
#13267=CLOSED_SHELL('',(#12588,#12589,#12590,#12591,#12592,#12593,#12594,
#12595,#12596,#12597,#12598,#12599,#12600,#12601));
#13268=CLOSED_SHELL('',(#12602,#12603,#12604,#12605,#12606,#12607,#12608,
#12609,#12610,#12611,#12612,#12613,#12614,#12615,#12616,#12617,#12618,#12619));
#13269=CLOSED_SHELL('',(#12620,#12621,#12622,#12623,#12624,#12625,#12626,
#12627,#12628,#12629,#12630,#12631,#12632,#12633,#12634,#12635));
#13270=CLOSED_SHELL('',(#12636,#12637,#12638));
#13271=CLOSED_SHELL('',(#12639,#12640,#12641));
#13272=CLOSED_SHELL('',(#12642,#12643,#12644,#12645,#12646,#12647,#12648));
#13273=CLOSED_SHELL('',(#12649,#12650,#12651,#12652));
#13274=CLOSED_SHELL('',(#12653,#12654,#12655,#12656));
#13275=CLOSED_SHELL('',(#12657,#12658,#12659,#12660));
#13276=CLOSED_SHELL('',(#12661,#12662,#12663,#12664));
#13277=CLOSED_SHELL('',(#12665,#12666,#12667,#12668));
#13278=CLOSED_SHELL('',(#12669,#12670,#12671,#12672));
#13279=CLOSED_SHELL('',(#12673,#12674,#12675,#12676,#12677,#12678,#12679,
#12680,#12681));
#13280=CLOSED_SHELL('',(#12682,#12683,#12684,#12685,#12686,#12687,#12688,
#12689));
#13281=CLOSED_SHELL('',(#12690,#12691,#12692,#12693,#12694,#12695,#12696,
#12697,#12698));
#13282=CLOSED_SHELL('',(#12699,#12700,#12701,#12702,#12703,#12704,#12705,
#12706,#12707,#12708,#12709,#12710,#12711));
#13283=CLOSED_SHELL('',(#12712,#12713,#12714,#12715,#12716,#12717,#12718,
#12719,#12720,#12721,#12722,#12723,#12724));
#13284=CLOSED_SHELL('',(#12725,#12726,#12727,#12728,#12729,#12730,#12731,
#12732,#12733,#12734));
#13285=CLOSED_SHELL('',(#12735,#12736,#12737,#12738,#12739,#12740,#12741));
#13286=CLOSED_SHELL('',(#12742,#12743,#12744,#12745));
#13287=CLOSED_SHELL('',(#12746,#12747,#12748,#12749));
#13288=CLOSED_SHELL('',(#12750,#12751,#12752,#12753));
#13289=CLOSED_SHELL('',(#12754,#12755,#12756,#12757));
#13290=CLOSED_SHELL('',(#12758,#12759,#12760,#12761));
#13291=CLOSED_SHELL('',(#12762,#12763,#12764,#12765));
#13292=CLOSED_SHELL('',(#12766,#12767,#12768,#12769,#12770,#12771,#12772,
#12773,#12774));
#13293=CLOSED_SHELL('',(#12775,#12776,#12777,#12778,#12779,#12780,#12781,
#12782,#12783,#12784,#12785,#12786,#12787));
#13294=CLOSED_SHELL('',(#12788,#12789,#12790,#12791,#12792,#12793,#12794,
#12795,#12796,#12797,#12798,#12799,#12800));
#13295=CLOSED_SHELL('',(#12801,#12802,#12803,#12804,#12805,#12806,#12807,
#12808,#12809,#12810));
#13296=CLOSED_SHELL('',(#12811,#12812,#12813,#12814,#12815,#12816,#12817));
#13297=CLOSED_SHELL('',(#12818,#12819,#12820,#12821));
#13298=CLOSED_SHELL('',(#12822,#12823,#12824,#12825));
#13299=CLOSED_SHELL('',(#12826,#12827,#12828,#12829));
#13300=CLOSED_SHELL('',(#12830,#12831,#12832,#12833));
#13301=CLOSED_SHELL('',(#12834,#12835,#12836,#12837));
#13302=CLOSED_SHELL('',(#12838,#12839,#12840,#12841));
#13303=CLOSED_SHELL('',(#12842,#12843,#12844,#12845,#12846,#12847,#12848,
#12849,#12850,#12851,#12852,#12853,#12854,#12855,#12856,#12857,#12858));
#13304=CLOSED_SHELL('',(#12859,#12860,#12861,#12862,#12863,#12864,#12865,
#12866));
#13305=CLOSED_SHELL('',(#12867,#12868,#12869,#12870,#12871,#12872,#12873,
#12874,#12875,#12876,#12877));
#13306=CLOSED_SHELL('',(#12878,#12879,#12880,#12881,#12882,#12883,#12884,
#12885,#12886,#12887,#12888,#12889,#12890));
#13307=CLOSED_SHELL('',(#12891,#12892,#12893,#12894));
#13308=CLOSED_SHELL('',(#12895,#12896,#12897,#12898));
#13309=CLOSED_SHELL('',(#12899,#12900,#12901,#12902));
#13310=CLOSED_SHELL('',(#12903,#12904,#12905,#12906,#12907,#12908,#12909,
#12910,#12911,#12912,#12913,#12914,#12915));
#13311=CLOSED_SHELL('',(#12916,#12917,#12918,#12919));
#13312=CLOSED_SHELL('',(#12920,#12921,#12922,#12923));
#13313=CLOSED_SHELL('',(#12924,#12925,#12926,#12927));
#13314=CLOSED_SHELL('',(#12928,#12929,#12930,#12931,#12932,#12933,#12934));
#13315=CLOSED_SHELL('',(#12935,#12936,#12937,#12938));
#13316=CLOSED_SHELL('',(#12939,#12940,#12941,#12942));
#13317=CLOSED_SHELL('',(#12943,#12944,#12945,#12946));
#13318=CLOSED_SHELL('',(#12947,#12948,#12949,#12950));
#13319=CLOSED_SHELL('',(#12951,#12952,#12953,#12954));
#13320=CLOSED_SHELL('',(#12955,#12956,#12957,#12958));
#13321=CLOSED_SHELL('',(#12959,#12960,#12961,#12962));
#13322=CLOSED_SHELL('',(#12963,#12964,#12965,#12966,#12967,#12968,#12969,
#12970,#12971));
#13323=CLOSED_SHELL('',(#12972,#12973,#12974,#12975,#12976,#12977,#12978,
#12979));
#13324=CLOSED_SHELL('',(#12980,#12981,#12982,#12983,#12984,#12985,#12986,
#12987,#12988,#12989,#12990,#12991,#12992,#12993,#12994,#12995,#12996));
#13325=CLOSED_SHELL('',(#12997,#12998,#12999,#13000));
#13326=CLOSED_SHELL('',(#13001,#13002,#13003,#13004));
#13327=CLOSED_SHELL('',(#13005,#13006,#13007,#13008,#13009,#13010,#13011,
#13012));
#13328=CLOSED_SHELL('',(#13013,#13014,#13015,#13016,#13017));
#13329=CLOSED_SHELL('',(#13018,#13019,#13020,#13021,#13022));
#13330=CLOSED_SHELL('',(#13023,#13024,#13025,#13026,#13027));
#13331=CLOSED_SHELL('',(#13028,#13029,#13030,#13031,#13032));
#13332=CLOSED_SHELL('',(#13033,#13034,#13035,#13036,#13037,#13038,#13039,
#13040));
#13333=CLOSED_SHELL('',(#13041,#13042,#13043,#13044,#13045));
#13334=CLOSED_SHELL('',(#13046,#13047,#13048,#13049,#13050));
#13335=CLOSED_SHELL('',(#13051,#13052,#13053,#13054,#13055));
#13336=CLOSED_SHELL('',(#13056,#13057,#13058,#13059,#13060));
#13337=CLOSED_SHELL('',(#13061,#13062,#13063,#13064,#13065,#13066,#13067,
#13068,#13069,#13070,#13071,#13072,#13073,#13074,#13075,#13076,#13077));
#13338=CLOSED_SHELL('',(#13078,#13079,#13080,#13081));
#13339=CLOSED_SHELL('',(#13082,#13083,#13084,#13085));
#13340=CLOSED_SHELL('',(#13086,#13087,#13088,#13089,#13090,#13091,#13092,
#13093));
#13341=CLOSED_SHELL('',(#13094,#13095,#13096,#13097,#13098));
#13342=CLOSED_SHELL('',(#13099,#13100,#13101,#13102,#13103));
#13343=CLOSED_SHELL('',(#13104,#13105,#13106,#13107,#13108));
#13344=CLOSED_SHELL('',(#13109,#13110,#13111,#13112,#13113));
#13345=CLOSED_SHELL('',(#13114,#13115,#13116,#13117,#13118,#13119,#13120,
#13121));
#13346=CLOSED_SHELL('',(#13122,#13123,#13124,#13125,#13126));
#13347=CLOSED_SHELL('',(#13127,#13128,#13129,#13130,#13131));
#13348=CLOSED_SHELL('',(#13132,#13133,#13134,#13135,#13136));
#13349=CLOSED_SHELL('',(#13137,#13138,#13139,#13140,#13141));
#13350=CLOSED_SHELL('',(#13142,#13143,#13144,#13145,#13146,#13147,#13148,
#13149));
#13351=CLOSED_SHELL('',(#13150,#13151,#13152,#13153,#13154,#13155,#13156,
#13157));
#13352=CLOSED_SHELL('',(#13158));
#13353=CLOSED_SHELL('',(#13159));
#13354=CLOSED_SHELL('',(#13160));
#13355=CLOSED_SHELL('',(#13161));
#13356=CLOSED_SHELL('',(#13162));
#13357=CLOSED_SHELL('',(#13163));
#13358=CLOSED_SHELL('',(#13164));
#13359=CLOSED_SHELL('',(#13165,#13166,#13167,#13168,#13169,#13170));
#13360=CLOSED_SHELL('',(#13171,#13172,#13173,#13174,#13175,#13176));
#13361=CLOSED_SHELL('',(#13177,#13178,#13179,#13180,#13181,#13182));
#13362=CLOSED_SHELL('',(#13183,#13184,#13185,#13186,#13187,#13188));
#13363=CLOSED_SHELL('',(#13189,#13190,#13191,#13192,#13193,#13194));
#13364=CLOSED_SHELL('',(#13195,#13196,#13197,#13198,#13199,#13200));
#13365=CLOSED_SHELL('',(#13201,#13202,#13203,#13204,#13205,#13206));
#13366=CLOSED_SHELL('',(#13207,#13208,#13209,#13210));
#13367=CLOSED_SHELL('',(#13211,#13212,#13213,#13214));
#13368=CLOSED_SHELL('',(#13215,#13216,#13217,#13218,#13219,#13220,#13221,
#13222,#13223,#13224,#13225));
#13369=CLOSED_SHELL('',(#13226,#13227,#13228,#13229));
#13370=CLOSED_SHELL('',(#13230,#13231,#13232,#13233));
#13371=CLOSED_SHELL('',(#13234,#13235,#13236,#13237));
#13372=CLOSED_SHELL('',(#13238,#13239,#13240,#13241));
#13373=CLOSED_SHELL('',(#13242,#13243,#13244,#13245,#13246,#13247));
#13374=DERIVED_UNIT_ELEMENT(#13594,1.);
#13375=DERIVED_UNIT_ELEMENT(#25102,-3.);
#13376=DERIVED_UNIT_ELEMENT(#13594,1.);
#13377=DERIVED_UNIT_ELEMENT(#25102,-3.);
#13378=DERIVED_UNIT_ELEMENT(#13594,1.);
#13379=DERIVED_UNIT_ELEMENT(#25102,-3.);
#13380=DERIVED_UNIT_ELEMENT(#13594,1.);
#13381=DERIVED_UNIT_ELEMENT(#25102,-3.);
#13382=DERIVED_UNIT_ELEMENT(#13594,1.);
#13383=DERIVED_UNIT_ELEMENT(#25102,-3.);
#13384=DERIVED_UNIT_ELEMENT(#13594,1.);
#13385=DERIVED_UNIT_ELEMENT(#25102,-3.);
#13386=DERIVED_UNIT_ELEMENT(#13594,1.);
#13387=DERIVED_UNIT_ELEMENT(#25102,-3.);
#13388=DERIVED_UNIT_ELEMENT(#13594,1.);
#13389=DERIVED_UNIT_ELEMENT(#25102,-3.);
#13390=DERIVED_UNIT_ELEMENT(#13594,1.);
#13391=DERIVED_UNIT_ELEMENT(#25102,-3.);
#13392=DERIVED_UNIT_ELEMENT(#13594,1.);
#13393=DERIVED_UNIT_ELEMENT(#25102,-3.);
#13394=DERIVED_UNIT_ELEMENT(#13594,1.);
#13395=DERIVED_UNIT_ELEMENT(#25102,-3.);
#13396=DERIVED_UNIT_ELEMENT(#13594,1.);
#13397=DERIVED_UNIT_ELEMENT(#25102,-3.);
#13398=DERIVED_UNIT_ELEMENT(#13594,1.);
#13399=DERIVED_UNIT_ELEMENT(#25102,-3.);
#13400=DERIVED_UNIT_ELEMENT(#13594,1.);
#13401=DERIVED_UNIT_ELEMENT(#25102,-3.);
#13402=DERIVED_UNIT_ELEMENT(#13594,1.);
#13403=DERIVED_UNIT_ELEMENT(#25102,-3.);
#13404=DERIVED_UNIT_ELEMENT(#13594,1.);
#13405=DERIVED_UNIT_ELEMENT(#25102,-3.);
#13406=DERIVED_UNIT_ELEMENT(#13594,1.);
#13407=DERIVED_UNIT_ELEMENT(#25102,-3.);
#13408=DERIVED_UNIT_ELEMENT(#13594,1.);
#13409=DERIVED_UNIT_ELEMENT(#25102,-3.);
#13410=DERIVED_UNIT_ELEMENT(#13594,1.);
#13411=DERIVED_UNIT_ELEMENT(#25102,-3.);
#13412=DERIVED_UNIT_ELEMENT(#13594,1.);
#13413=DERIVED_UNIT_ELEMENT(#25102,-3.);
#13414=DERIVED_UNIT_ELEMENT(#13594,1.);
#13415=DERIVED_UNIT_ELEMENT(#25102,-3.);
#13416=DERIVED_UNIT_ELEMENT(#13594,1.);
#13417=DERIVED_UNIT_ELEMENT(#25102,-3.);
#13418=DERIVED_UNIT_ELEMENT(#13594,1.);
#13419=DERIVED_UNIT_ELEMENT(#25102,-3.);
#13420=DERIVED_UNIT_ELEMENT(#13594,1.);
#13421=DERIVED_UNIT_ELEMENT(#25102,-3.);
#13422=DERIVED_UNIT_ELEMENT(#13594,1.);
#13423=DERIVED_UNIT_ELEMENT(#25102,-3.);
#13424=DERIVED_UNIT_ELEMENT(#13594,1.);
#13425=DERIVED_UNIT_ELEMENT(#25102,-3.);
#13426=DERIVED_UNIT_ELEMENT(#13594,1.);
#13427=DERIVED_UNIT_ELEMENT(#25102,-3.);
#13428=DERIVED_UNIT_ELEMENT(#13594,1.);
#13429=DERIVED_UNIT_ELEMENT(#25102,-3.);
#13430=DERIVED_UNIT_ELEMENT(#13594,1.);
#13431=DERIVED_UNIT_ELEMENT(#25102,-3.);
#13432=DERIVED_UNIT_ELEMENT(#13594,1.);
#13433=DERIVED_UNIT_ELEMENT(#25102,-3.);
#13434=DERIVED_UNIT_ELEMENT(#13594,1.);
#13435=DERIVED_UNIT_ELEMENT(#25102,-3.);
#13436=DERIVED_UNIT_ELEMENT(#13594,1.);
#13437=DERIVED_UNIT_ELEMENT(#25102,-3.);
#13438=DERIVED_UNIT_ELEMENT(#13594,1.);
#13439=DERIVED_UNIT_ELEMENT(#25102,-3.);
#13440=DERIVED_UNIT_ELEMENT(#13594,1.);
#13441=DERIVED_UNIT_ELEMENT(#25102,-3.);
#13442=DERIVED_UNIT_ELEMENT(#13594,1.);
#13443=DERIVED_UNIT_ELEMENT(#25102,-3.);
#13444=DERIVED_UNIT_ELEMENT(#13594,1.);
#13445=DERIVED_UNIT_ELEMENT(#25102,-3.);
#13446=DERIVED_UNIT_ELEMENT(#13594,1.);
#13447=DERIVED_UNIT_ELEMENT(#25102,-3.);
#13448=DERIVED_UNIT_ELEMENT(#13594,1.);
#13449=DERIVED_UNIT_ELEMENT(#25102,-3.);
#13450=DERIVED_UNIT_ELEMENT(#13594,1.);
#13451=DERIVED_UNIT_ELEMENT(#25102,-3.);
#13452=DERIVED_UNIT_ELEMENT(#13594,1.);
#13453=DERIVED_UNIT_ELEMENT(#25102,-3.);
#13454=DERIVED_UNIT_ELEMENT(#13594,1.);
#13455=DERIVED_UNIT_ELEMENT(#25102,-3.);
#13456=DERIVED_UNIT_ELEMENT(#13594,1.);
#13457=DERIVED_UNIT_ELEMENT(#25102,-3.);
#13458=DERIVED_UNIT_ELEMENT(#13594,1.);
#13459=DERIVED_UNIT_ELEMENT(#25102,-3.);
#13460=DERIVED_UNIT_ELEMENT(#13594,1.);
#13461=DERIVED_UNIT_ELEMENT(#25102,-3.);
#13462=DERIVED_UNIT_ELEMENT(#13594,1.);
#13463=DERIVED_UNIT_ELEMENT(#25102,-3.);
#13464=DERIVED_UNIT_ELEMENT(#13594,1.);
#13465=DERIVED_UNIT_ELEMENT(#25102,-3.);
#13466=DERIVED_UNIT_ELEMENT(#13594,1.);
#13467=DERIVED_UNIT_ELEMENT(#25102,-3.);
#13468=DERIVED_UNIT_ELEMENT(#13594,1.);
#13469=DERIVED_UNIT_ELEMENT(#25102,-3.);
#13470=DERIVED_UNIT_ELEMENT(#13594,1.);
#13471=DERIVED_UNIT_ELEMENT(#25102,-3.);
#13472=DERIVED_UNIT_ELEMENT(#13594,1.);
#13473=DERIVED_UNIT_ELEMENT(#25102,-3.);
#13474=DERIVED_UNIT_ELEMENT(#13594,1.);
#13475=DERIVED_UNIT_ELEMENT(#25102,-3.);
#13476=DERIVED_UNIT_ELEMENT(#13594,1.);
#13477=DERIVED_UNIT_ELEMENT(#25102,-3.);
#13478=DERIVED_UNIT_ELEMENT(#13594,1.);
#13479=DERIVED_UNIT_ELEMENT(#25102,-3.);
#13480=DERIVED_UNIT_ELEMENT(#13594,1.);
#13481=DERIVED_UNIT_ELEMENT(#25102,-3.);
#13482=DERIVED_UNIT_ELEMENT(#13594,1.);
#13483=DERIVED_UNIT_ELEMENT(#25102,-3.);
#13484=DERIVED_UNIT_ELEMENT(#13594,1.);
#13485=DERIVED_UNIT_ELEMENT(#25102,-3.);
#13486=DERIVED_UNIT_ELEMENT(#13594,1.);
#13487=DERIVED_UNIT_ELEMENT(#25102,-3.);
#13488=DERIVED_UNIT_ELEMENT(#13594,1.);
#13489=DERIVED_UNIT_ELEMENT(#25102,-3.);
#13490=DERIVED_UNIT_ELEMENT(#13594,1.);
#13491=DERIVED_UNIT_ELEMENT(#25102,-3.);
#13492=DERIVED_UNIT_ELEMENT(#13594,1.);
#13493=DERIVED_UNIT_ELEMENT(#25102,-3.);
#13494=DERIVED_UNIT_ELEMENT(#13594,1.);
#13495=DERIVED_UNIT_ELEMENT(#25102,-3.);
#13496=DERIVED_UNIT_ELEMENT(#13594,1.);
#13497=DERIVED_UNIT_ELEMENT(#25102,-3.);
#13498=DERIVED_UNIT_ELEMENT(#13594,1.);
#13499=DERIVED_UNIT_ELEMENT(#25102,-3.);
#13500=DERIVED_UNIT_ELEMENT(#13594,1.);
#13501=DERIVED_UNIT_ELEMENT(#25102,-3.);
#13502=DERIVED_UNIT_ELEMENT(#13594,1.);
#13503=DERIVED_UNIT_ELEMENT(#25102,-3.);
#13504=DERIVED_UNIT_ELEMENT(#13594,1.);
#13505=DERIVED_UNIT_ELEMENT(#25102,-3.);
#13506=DERIVED_UNIT_ELEMENT(#13594,1.);
#13507=DERIVED_UNIT_ELEMENT(#25102,-3.);
#13508=DERIVED_UNIT_ELEMENT(#13594,1.);
#13509=DERIVED_UNIT_ELEMENT(#25102,-3.);
#13510=DERIVED_UNIT_ELEMENT(#13594,1.);
#13511=DERIVED_UNIT_ELEMENT(#25102,-3.);
#13512=DERIVED_UNIT_ELEMENT(#13594,1.);
#13513=DERIVED_UNIT_ELEMENT(#25102,-3.);
#13514=DERIVED_UNIT_ELEMENT(#13594,1.);
#13515=DERIVED_UNIT_ELEMENT(#25102,-3.);
#13516=DERIVED_UNIT_ELEMENT(#13594,1.);
#13517=DERIVED_UNIT_ELEMENT(#25102,-3.);
#13518=DERIVED_UNIT_ELEMENT(#13594,1.);
#13519=DERIVED_UNIT_ELEMENT(#25102,-3.);
#13520=DERIVED_UNIT_ELEMENT(#13594,1.);
#13521=DERIVED_UNIT_ELEMENT(#25102,-3.);
#13522=DERIVED_UNIT_ELEMENT(#13594,1.);
#13523=DERIVED_UNIT_ELEMENT(#25102,-3.);
#13524=DERIVED_UNIT_ELEMENT(#13594,1.);
#13525=DERIVED_UNIT_ELEMENT(#25102,-3.);
#13526=DERIVED_UNIT_ELEMENT(#13594,1.);
#13527=DERIVED_UNIT_ELEMENT(#25102,-3.);
#13528=DERIVED_UNIT_ELEMENT(#13594,1.);
#13529=DERIVED_UNIT_ELEMENT(#25102,-3.);
#13530=DERIVED_UNIT_ELEMENT(#13594,1.);
#13531=DERIVED_UNIT_ELEMENT(#25102,-3.);
#13532=DERIVED_UNIT_ELEMENT(#13594,1.);
#13533=DERIVED_UNIT_ELEMENT(#25102,-3.);
#13534=DERIVED_UNIT_ELEMENT(#13594,1.);
#13535=DERIVED_UNIT_ELEMENT(#25102,-3.);
#13536=DERIVED_UNIT_ELEMENT(#13594,1.);
#13537=DERIVED_UNIT_ELEMENT(#25102,-3.);
#13538=DERIVED_UNIT_ELEMENT(#13594,1.);
#13539=DERIVED_UNIT_ELEMENT(#25102,-3.);
#13540=DERIVED_UNIT_ELEMENT(#13594,1.);
#13541=DERIVED_UNIT_ELEMENT(#25102,-3.);
#13542=DERIVED_UNIT_ELEMENT(#13594,1.);
#13543=DERIVED_UNIT_ELEMENT(#25102,-3.);
#13544=DERIVED_UNIT_ELEMENT(#13594,1.);
#13545=DERIVED_UNIT_ELEMENT(#25102,-3.);
#13546=DERIVED_UNIT_ELEMENT(#13594,1.);
#13547=DERIVED_UNIT_ELEMENT(#25102,-3.);
#13548=DERIVED_UNIT_ELEMENT(#13594,1.);
#13549=DERIVED_UNIT_ELEMENT(#25102,-3.);
#13550=DERIVED_UNIT_ELEMENT(#13594,1.);
#13551=DERIVED_UNIT_ELEMENT(#25102,-3.);
#13552=DERIVED_UNIT_ELEMENT(#13594,1.);
#13553=DERIVED_UNIT_ELEMENT(#25102,-3.);
#13554=DERIVED_UNIT_ELEMENT(#13594,1.);
#13555=DERIVED_UNIT_ELEMENT(#25102,-3.);
#13556=DERIVED_UNIT_ELEMENT(#13594,1.);
#13557=DERIVED_UNIT_ELEMENT(#25102,-3.);
#13558=DERIVED_UNIT_ELEMENT(#13594,1.);
#13559=DERIVED_UNIT_ELEMENT(#25102,-3.);
#13560=DERIVED_UNIT_ELEMENT(#13594,1.);
#13561=DERIVED_UNIT_ELEMENT(#25102,-3.);
#13562=DERIVED_UNIT_ELEMENT(#13594,1.);
#13563=DERIVED_UNIT_ELEMENT(#25102,-3.);
#13564=DERIVED_UNIT_ELEMENT(#13594,1.);
#13565=DERIVED_UNIT_ELEMENT(#25102,-3.);
#13566=DERIVED_UNIT_ELEMENT(#13594,1.);
#13567=DERIVED_UNIT_ELEMENT(#25102,-3.);
#13568=DERIVED_UNIT_ELEMENT(#13594,1.);
#13569=DERIVED_UNIT_ELEMENT(#25102,-3.);
#13570=DERIVED_UNIT_ELEMENT(#13594,1.);
#13571=DERIVED_UNIT_ELEMENT(#25102,-3.);
#13572=DERIVED_UNIT_ELEMENT(#13594,1.);
#13573=DERIVED_UNIT_ELEMENT(#25102,-3.);
#13574=DERIVED_UNIT_ELEMENT(#13594,1.);
#13575=DERIVED_UNIT_ELEMENT(#25102,-3.);
#13576=DERIVED_UNIT_ELEMENT(#13594,1.);
#13577=DERIVED_UNIT_ELEMENT(#25102,-3.);
#13578=DERIVED_UNIT_ELEMENT(#13594,1.);
#13579=DERIVED_UNIT_ELEMENT(#25102,-3.);
#13580=DERIVED_UNIT_ELEMENT(#13594,1.);
#13581=DERIVED_UNIT_ELEMENT(#25102,-3.);
#13582=DERIVED_UNIT_ELEMENT(#13594,1.);
#13583=DERIVED_UNIT_ELEMENT(#25102,-3.);
#13584=DERIVED_UNIT_ELEMENT(#13594,1.);
#13585=DERIVED_UNIT_ELEMENT(#25102,-3.);
#13586=DERIVED_UNIT_ELEMENT(#13594,1.);
#13587=DERIVED_UNIT_ELEMENT(#25102,-3.);
#13588=DERIVED_UNIT_ELEMENT(#13594,1.);
#13589=DERIVED_UNIT_ELEMENT(#25102,-3.);
#13590=DERIVED_UNIT_ELEMENT(#13594,1.);
#13591=DERIVED_UNIT_ELEMENT(#25102,-3.);
#13592=DERIVED_UNIT_ELEMENT(#13594,1.);
#13593=DERIVED_UNIT_ELEMENT(#25102,-3.);
#13594=(
MASS_UNIT()
NAMED_UNIT(*)
SI_UNIT(.KILO.,.GRAM.)
);
#13595=DERIVED_UNIT((#13374,#13375));
#13596=DERIVED_UNIT((#13376,#13377));
#13597=DERIVED_UNIT((#13378,#13379));
#13598=DERIVED_UNIT((#13380,#13381));
#13599=DERIVED_UNIT((#13382,#13383));
#13600=DERIVED_UNIT((#13384,#13385));
#13601=DERIVED_UNIT((#13386,#13387));
#13602=DERIVED_UNIT((#13388,#13389));
#13603=DERIVED_UNIT((#13390,#13391));
#13604=DERIVED_UNIT((#13392,#13393));
#13605=DERIVED_UNIT((#13394,#13395));
#13606=DERIVED_UNIT((#13396,#13397));
#13607=DERIVED_UNIT((#13398,#13399));
#13608=DERIVED_UNIT((#13400,#13401));
#13609=DERIVED_UNIT((#13402,#13403));
#13610=DERIVED_UNIT((#13404,#13405));
#13611=DERIVED_UNIT((#13406,#13407));
#13612=DERIVED_UNIT((#13408,#13409));
#13613=DERIVED_UNIT((#13410,#13411));
#13614=DERIVED_UNIT((#13412,#13413));
#13615=DERIVED_UNIT((#13414,#13415));
#13616=DERIVED_UNIT((#13416,#13417));
#13617=DERIVED_UNIT((#13418,#13419));
#13618=DERIVED_UNIT((#13420,#13421));
#13619=DERIVED_UNIT((#13422,#13423));
#13620=DERIVED_UNIT((#13424,#13425));
#13621=DERIVED_UNIT((#13426,#13427));
#13622=DERIVED_UNIT((#13428,#13429));
#13623=DERIVED_UNIT((#13430,#13431));
#13624=DERIVED_UNIT((#13432,#13433));
#13625=DERIVED_UNIT((#13434,#13435));
#13626=DERIVED_UNIT((#13436,#13437));
#13627=DERIVED_UNIT((#13438,#13439));
#13628=DERIVED_UNIT((#13440,#13441));
#13629=DERIVED_UNIT((#13442,#13443));
#13630=DERIVED_UNIT((#13444,#13445));
#13631=DERIVED_UNIT((#13446,#13447));
#13632=DERIVED_UNIT((#13448,#13449));
#13633=DERIVED_UNIT((#13450,#13451));
#13634=DERIVED_UNIT((#13452,#13453));
#13635=DERIVED_UNIT((#13454,#13455));
#13636=DERIVED_UNIT((#13456,#13457));
#13637=DERIVED_UNIT((#13458,#13459));
#13638=DERIVED_UNIT((#13460,#13461));
#13639=DERIVED_UNIT((#13462,#13463));
#13640=DERIVED_UNIT((#13464,#13465));
#13641=DERIVED_UNIT((#13466,#13467));
#13642=DERIVED_UNIT((#13468,#13469));
#13643=DERIVED_UNIT((#13470,#13471));
#13644=DERIVED_UNIT((#13472,#13473));
#13645=DERIVED_UNIT((#13474,#13475));
#13646=DERIVED_UNIT((#13476,#13477));
#13647=DERIVED_UNIT((#13478,#13479));
#13648=DERIVED_UNIT((#13480,#13481));
#13649=DERIVED_UNIT((#13482,#13483));
#13650=DERIVED_UNIT((#13484,#13485));
#13651=DERIVED_UNIT((#13486,#13487));
#13652=DERIVED_UNIT((#13488,#13489));
#13653=DERIVED_UNIT((#13490,#13491));
#13654=DERIVED_UNIT((#13492,#13493));
#13655=DERIVED_UNIT((#13494,#13495));
#13656=DERIVED_UNIT((#13496,#13497));
#13657=DERIVED_UNIT((#13498,#13499));
#13658=DERIVED_UNIT((#13500,#13501));
#13659=DERIVED_UNIT((#13502,#13503));
#13660=DERIVED_UNIT((#13504,#13505));
#13661=DERIVED_UNIT((#13506,#13507));
#13662=DERIVED_UNIT((#13508,#13509));
#13663=DERIVED_UNIT((#13510,#13511));
#13664=DERIVED_UNIT((#13512,#13513));
#13665=DERIVED_UNIT((#13514,#13515));
#13666=DERIVED_UNIT((#13516,#13517));
#13667=DERIVED_UNIT((#13518,#13519));
#13668=DERIVED_UNIT((#13520,#13521));
#13669=DERIVED_UNIT((#13522,#13523));
#13670=DERIVED_UNIT((#13524,#13525));
#13671=DERIVED_UNIT((#13526,#13527));
#13672=DERIVED_UNIT((#13528,#13529));
#13673=DERIVED_UNIT((#13530,#13531));
#13674=DERIVED_UNIT((#13532,#13533));
#13675=DERIVED_UNIT((#13534,#13535));
#13676=DERIVED_UNIT((#13536,#13537));
#13677=DERIVED_UNIT((#13538,#13539));
#13678=DERIVED_UNIT((#13540,#13541));
#13679=DERIVED_UNIT((#13542,#13543));
#13680=DERIVED_UNIT((#13544,#13545));
#13681=DERIVED_UNIT((#13546,#13547));
#13682=DERIVED_UNIT((#13548,#13549));
#13683=DERIVED_UNIT((#13550,#13551));
#13684=DERIVED_UNIT((#13552,#13553));
#13685=DERIVED_UNIT((#13554,#13555));
#13686=DERIVED_UNIT((#13556,#13557));
#13687=DERIVED_UNIT((#13558,#13559));
#13688=DERIVED_UNIT((#13560,#13561));
#13689=DERIVED_UNIT((#13562,#13563));
#13690=DERIVED_UNIT((#13564,#13565));
#13691=DERIVED_UNIT((#13566,#13567));
#13692=DERIVED_UNIT((#13568,#13569));
#13693=DERIVED_UNIT((#13570,#13571));
#13694=DERIVED_UNIT((#13572,#13573));
#13695=DERIVED_UNIT((#13574,#13575));
#13696=DERIVED_UNIT((#13576,#13577));
#13697=DERIVED_UNIT((#13578,#13579));
#13698=DERIVED_UNIT((#13580,#13581));
#13699=DERIVED_UNIT((#13582,#13583));
#13700=DERIVED_UNIT((#13584,#13585));
#13701=DERIVED_UNIT((#13586,#13587));
#13702=DERIVED_UNIT((#13588,#13589));
#13703=DERIVED_UNIT((#13590,#13591));
#13704=DERIVED_UNIT((#13592,#13593));
#13705=MEASURE_REPRESENTATION_ITEM('density measure',
POSITIVE_RATIO_MEASURE(7850.),#13595);
#13706=MEASURE_REPRESENTATION_ITEM('density measure',
POSITIVE_RATIO_MEASURE(7850.),#13596);
#13707=MEASURE_REPRESENTATION_ITEM('density measure',
POSITIVE_RATIO_MEASURE(7850.),#13597);
#13708=MEASURE_REPRESENTATION_ITEM('density measure',
POSITIVE_RATIO_MEASURE(7850.),#13598);
#13709=MEASURE_REPRESENTATION_ITEM('density measure',
POSITIVE_RATIO_MEASURE(7850.),#13599);
#13710=MEASURE_REPRESENTATION_ITEM('density measure',
POSITIVE_RATIO_MEASURE(7850.),#13600);
#13711=MEASURE_REPRESENTATION_ITEM('density measure',
POSITIVE_RATIO_MEASURE(7850.),#13601);
#13712=MEASURE_REPRESENTATION_ITEM('density measure',
POSITIVE_RATIO_MEASURE(7850.),#13602);
#13713=MEASURE_REPRESENTATION_ITEM('density measure',
POSITIVE_RATIO_MEASURE(7850.),#13603);
#13714=MEASURE_REPRESENTATION_ITEM('density measure',
POSITIVE_RATIO_MEASURE(7850.),#13604);
#13715=MEASURE_REPRESENTATION_ITEM('density measure',
POSITIVE_RATIO_MEASURE(7850.),#13605);
#13716=MEASURE_REPRESENTATION_ITEM('density measure',
POSITIVE_RATIO_MEASURE(7850.),#13606);
#13717=MEASURE_REPRESENTATION_ITEM('density measure',
POSITIVE_RATIO_MEASURE(7850.),#13607);
#13718=MEASURE_REPRESENTATION_ITEM('density measure',
POSITIVE_RATIO_MEASURE(7850.),#13608);
#13719=MEASURE_REPRESENTATION_ITEM('density measure',
POSITIVE_RATIO_MEASURE(7850.),#13609);
#13720=MEASURE_REPRESENTATION_ITEM('density measure',
POSITIVE_RATIO_MEASURE(7850.),#13610);
#13721=MEASURE_REPRESENTATION_ITEM('density measure',
POSITIVE_RATIO_MEASURE(7850.),#13611);
#13722=MEASURE_REPRESENTATION_ITEM('density measure',
POSITIVE_RATIO_MEASURE(7850.),#13612);
#13723=MEASURE_REPRESENTATION_ITEM('density measure',
POSITIVE_RATIO_MEASURE(7850.),#13613);
#13724=MEASURE_REPRESENTATION_ITEM('density measure',
POSITIVE_RATIO_MEASURE(7850.),#13614);
#13725=MEASURE_REPRESENTATION_ITEM('density measure',
POSITIVE_RATIO_MEASURE(7850.),#13615);
#13726=MEASURE_REPRESENTATION_ITEM('density measure',
POSITIVE_RATIO_MEASURE(7850.),#13616);
#13727=MEASURE_REPRESENTATION_ITEM('density measure',
POSITIVE_RATIO_MEASURE(7850.),#13617);
#13728=MEASURE_REPRESENTATION_ITEM('density measure',
POSITIVE_RATIO_MEASURE(7850.),#13618);
#13729=MEASURE_REPRESENTATION_ITEM('density measure',
POSITIVE_RATIO_MEASURE(7850.),#13619);
#13730=MEASURE_REPRESENTATION_ITEM('density measure',
POSITIVE_RATIO_MEASURE(7850.),#13620);
#13731=MEASURE_REPRESENTATION_ITEM('density measure',
POSITIVE_RATIO_MEASURE(7850.),#13621);
#13732=MEASURE_REPRESENTATION_ITEM('density measure',
POSITIVE_RATIO_MEASURE(7850.),#13622);
#13733=MEASURE_REPRESENTATION_ITEM('density measure',
POSITIVE_RATIO_MEASURE(7850.),#13623);
#13734=MEASURE_REPRESENTATION_ITEM('density measure',
POSITIVE_RATIO_MEASURE(7850.),#13624);
#13735=MEASURE_REPRESENTATION_ITEM('density measure',
POSITIVE_RATIO_MEASURE(7850.),#13625);
#13736=MEASURE_REPRESENTATION_ITEM('density measure',
POSITIVE_RATIO_MEASURE(7850.),#13626);
#13737=MEASURE_REPRESENTATION_ITEM('density measure',
POSITIVE_RATIO_MEASURE(7850.),#13627);
#13738=MEASURE_REPRESENTATION_ITEM('density measure',
POSITIVE_RATIO_MEASURE(7850.),#13628);
#13739=MEASURE_REPRESENTATION_ITEM('density measure',
POSITIVE_RATIO_MEASURE(7850.),#13629);
#13740=MEASURE_REPRESENTATION_ITEM('density measure',
POSITIVE_RATIO_MEASURE(7850.),#13630);
#13741=MEASURE_REPRESENTATION_ITEM('density measure',
POSITIVE_RATIO_MEASURE(7850.),#13631);
#13742=MEASURE_REPRESENTATION_ITEM('density measure',
POSITIVE_RATIO_MEASURE(7850.),#13632);
#13743=MEASURE_REPRESENTATION_ITEM('density measure',
POSITIVE_RATIO_MEASURE(7850.),#13633);
#13744=MEASURE_REPRESENTATION_ITEM('density measure',
POSITIVE_RATIO_MEASURE(7850.),#13634);
#13745=MEASURE_REPRESENTATION_ITEM('density measure',
POSITIVE_RATIO_MEASURE(7850.),#13635);
#13746=MEASURE_REPRESENTATION_ITEM('density measure',
POSITIVE_RATIO_MEASURE(7850.),#13636);
#13747=MEASURE_REPRESENTATION_ITEM('density measure',
POSITIVE_RATIO_MEASURE(7850.),#13637);
#13748=MEASURE_REPRESENTATION_ITEM('density measure',
POSITIVE_RATIO_MEASURE(7850.),#13638);
#13749=MEASURE_REPRESENTATION_ITEM('density measure',
POSITIVE_RATIO_MEASURE(7850.),#13639);
#13750=MEASURE_REPRESENTATION_ITEM('density measure',
POSITIVE_RATIO_MEASURE(7850.),#13640);
#13751=MEASURE_REPRESENTATION_ITEM('density measure',
POSITIVE_RATIO_MEASURE(7850.),#13641);
#13752=MEASURE_REPRESENTATION_ITEM('density measure',
POSITIVE_RATIO_MEASURE(7850.),#13642);
#13753=MEASURE_REPRESENTATION_ITEM('density measure',
POSITIVE_RATIO_MEASURE(7850.),#13643);
#13754=MEASURE_REPRESENTATION_ITEM('density measure',
POSITIVE_RATIO_MEASURE(7850.),#13644);
#13755=MEASURE_REPRESENTATION_ITEM('density measure',
POSITIVE_RATIO_MEASURE(7850.),#13645);
#13756=MEASURE_REPRESENTATION_ITEM('density measure',
POSITIVE_RATIO_MEASURE(7850.),#13646);
#13757=MEASURE_REPRESENTATION_ITEM('density measure',
POSITIVE_RATIO_MEASURE(7850.),#13647);
#13758=MEASURE_REPRESENTATION_ITEM('density measure',
POSITIVE_RATIO_MEASURE(7850.),#13648);
#13759=MEASURE_REPRESENTATION_ITEM('density measure',
POSITIVE_RATIO_MEASURE(7850.),#13649);
#13760=MEASURE_REPRESENTATION_ITEM('density measure',
POSITIVE_RATIO_MEASURE(7850.),#13650);
#13761=MEASURE_REPRESENTATION_ITEM('density measure',
POSITIVE_RATIO_MEASURE(7850.),#13651);
#13762=MEASURE_REPRESENTATION_ITEM('density measure',
POSITIVE_RATIO_MEASURE(7850.),#13652);
#13763=MEASURE_REPRESENTATION_ITEM('density measure',
POSITIVE_RATIO_MEASURE(7850.),#13653);
#13764=MEASURE_REPRESENTATION_ITEM('density measure',
POSITIVE_RATIO_MEASURE(7850.),#13654);
#13765=MEASURE_REPRESENTATION_ITEM('density measure',
POSITIVE_RATIO_MEASURE(7850.),#13655);
#13766=MEASURE_REPRESENTATION_ITEM('density measure',
POSITIVE_RATIO_MEASURE(7850.),#13656);
#13767=MEASURE_REPRESENTATION_ITEM('density measure',
POSITIVE_RATIO_MEASURE(7850.),#13657);
#13768=MEASURE_REPRESENTATION_ITEM('density measure',
POSITIVE_RATIO_MEASURE(7850.),#13658);
#13769=MEASURE_REPRESENTATION_ITEM('density measure',
POSITIVE_RATIO_MEASURE(7850.),#13659);
#13770=MEASURE_REPRESENTATION_ITEM('density measure',
POSITIVE_RATIO_MEASURE(7850.),#13660);
#13771=MEASURE_REPRESENTATION_ITEM('density measure',
POSITIVE_RATIO_MEASURE(7850.),#13661);
#13772=MEASURE_REPRESENTATION_ITEM('density measure',
POSITIVE_RATIO_MEASURE(7850.),#13662);
#13773=MEASURE_REPRESENTATION_ITEM('density measure',
POSITIVE_RATIO_MEASURE(7850.),#13663);
#13774=MEASURE_REPRESENTATION_ITEM('density measure',
POSITIVE_RATIO_MEASURE(7850.),#13664);
#13775=MEASURE_REPRESENTATION_ITEM('density measure',
POSITIVE_RATIO_MEASURE(7850.),#13665);
#13776=MEASURE_REPRESENTATION_ITEM('density measure',
POSITIVE_RATIO_MEASURE(7850.),#13666);
#13777=MEASURE_REPRESENTATION_ITEM('density measure',
POSITIVE_RATIO_MEASURE(7850.),#13667);
#13778=MEASURE_REPRESENTATION_ITEM('density measure',
POSITIVE_RATIO_MEASURE(7850.),#13668);
#13779=MEASURE_REPRESENTATION_ITEM('density measure',
POSITIVE_RATIO_MEASURE(7850.),#13669);
#13780=MEASURE_REPRESENTATION_ITEM('density measure',
POSITIVE_RATIO_MEASURE(7850.),#13670);
#13781=MEASURE_REPRESENTATION_ITEM('density measure',
POSITIVE_RATIO_MEASURE(7850.),#13671);
#13782=MEASURE_REPRESENTATION_ITEM('density measure',
POSITIVE_RATIO_MEASURE(7850.),#13672);
#13783=MEASURE_REPRESENTATION_ITEM('density measure',
POSITIVE_RATIO_MEASURE(7850.),#13673);
#13784=MEASURE_REPRESENTATION_ITEM('density measure',
POSITIVE_RATIO_MEASURE(7850.),#13674);
#13785=MEASURE_REPRESENTATION_ITEM('density measure',
POSITIVE_RATIO_MEASURE(7850.),#13675);
#13786=MEASURE_REPRESENTATION_ITEM('density measure',
POSITIVE_RATIO_MEASURE(7850.),#13676);
#13787=MEASURE_REPRESENTATION_ITEM('density measure',
POSITIVE_RATIO_MEASURE(7850.),#13677);
#13788=MEASURE_REPRESENTATION_ITEM('density measure',
POSITIVE_RATIO_MEASURE(7850.),#13678);
#13789=MEASURE_REPRESENTATION_ITEM('density measure',
POSITIVE_RATIO_MEASURE(7850.),#13679);
#13790=MEASURE_REPRESENTATION_ITEM('density measure',
POSITIVE_RATIO_MEASURE(7850.),#13680);
#13791=MEASURE_REPRESENTATION_ITEM('density measure',
POSITIVE_RATIO_MEASURE(7850.),#13681);
#13792=MEASURE_REPRESENTATION_ITEM('density measure',
POSITIVE_RATIO_MEASURE(7850.),#13682);
#13793=MEASURE_REPRESENTATION_ITEM('density measure',
POSITIVE_RATIO_MEASURE(7850.),#13683);
#13794=MEASURE_REPRESENTATION_ITEM('density measure',
POSITIVE_RATIO_MEASURE(7850.),#13684);
#13795=MEASURE_REPRESENTATION_ITEM('density measure',
POSITIVE_RATIO_MEASURE(7850.),#13685);
#13796=MEASURE_REPRESENTATION_ITEM('density measure',
POSITIVE_RATIO_MEASURE(7850.),#13686);
#13797=MEASURE_REPRESENTATION_ITEM('density measure',
POSITIVE_RATIO_MEASURE(7850.),#13687);
#13798=MEASURE_REPRESENTATION_ITEM('density measure',
POSITIVE_RATIO_MEASURE(7850.),#13688);
#13799=MEASURE_REPRESENTATION_ITEM('density measure',
POSITIVE_RATIO_MEASURE(7850.),#13689);
#13800=MEASURE_REPRESENTATION_ITEM('density measure',
POSITIVE_RATIO_MEASURE(7850.),#13690);
#13801=MEASURE_REPRESENTATION_ITEM('density measure',
POSITIVE_RATIO_MEASURE(7850.),#13691);
#13802=MEASURE_REPRESENTATION_ITEM('density measure',
POSITIVE_RATIO_MEASURE(7850.),#13692);
#13803=MEASURE_REPRESENTATION_ITEM('density measure',
POSITIVE_RATIO_MEASURE(7850.),#13693);
#13804=MEASURE_REPRESENTATION_ITEM('density measure',
POSITIVE_RATIO_MEASURE(7850.),#13694);
#13805=MEASURE_REPRESENTATION_ITEM('density measure',
POSITIVE_RATIO_MEASURE(7850.),#13695);
#13806=MEASURE_REPRESENTATION_ITEM('density measure',
POSITIVE_RATIO_MEASURE(7850.),#13696);
#13807=MEASURE_REPRESENTATION_ITEM('density measure',
POSITIVE_RATIO_MEASURE(7850.),#13697);
#13808=MEASURE_REPRESENTATION_ITEM('density measure',
POSITIVE_RATIO_MEASURE(7850.),#13698);
#13809=MEASURE_REPRESENTATION_ITEM('density measure',
POSITIVE_RATIO_MEASURE(7850.),#13699);
#13810=MEASURE_REPRESENTATION_ITEM('density measure',
POSITIVE_RATIO_MEASURE(7850.),#13700);
#13811=MEASURE_REPRESENTATION_ITEM('density measure',
POSITIVE_RATIO_MEASURE(7850.),#13701);
#13812=MEASURE_REPRESENTATION_ITEM('density measure',
POSITIVE_RATIO_MEASURE(7850.),#13702);
#13813=MEASURE_REPRESENTATION_ITEM('density measure',
POSITIVE_RATIO_MEASURE(7850.),#13703);
#13814=MEASURE_REPRESENTATION_ITEM('density measure',
POSITIVE_RATIO_MEASURE(7850.),#13704);
#13815=PROPERTY_DEFINITION_REPRESENTATION(#14365,#14035);
#13816=PROPERTY_DEFINITION_REPRESENTATION(#14366,#14036);
#13817=PROPERTY_DEFINITION_REPRESENTATION(#14367,#14037);
#13818=PROPERTY_DEFINITION_REPRESENTATION(#14368,#14038);
#13819=PROPERTY_DEFINITION_REPRESENTATION(#14369,#14039);
#13820=PROPERTY_DEFINITION_REPRESENTATION(#14370,#14040);
#13821=PROPERTY_DEFINITION_REPRESENTATION(#14371,#14041);
#13822=PROPERTY_DEFINITION_REPRESENTATION(#14372,#14042);
#13823=PROPERTY_DEFINITION_REPRESENTATION(#14373,#14043);
#13824=PROPERTY_DEFINITION_REPRESENTATION(#14374,#14044);
#13825=PROPERTY_DEFINITION_REPRESENTATION(#14375,#14045);
#13826=PROPERTY_DEFINITION_REPRESENTATION(#14376,#14046);
#13827=PROPERTY_DEFINITION_REPRESENTATION(#14377,#14047);
#13828=PROPERTY_DEFINITION_REPRESENTATION(#14378,#14048);
#13829=PROPERTY_DEFINITION_REPRESENTATION(#14379,#14049);
#13830=PROPERTY_DEFINITION_REPRESENTATION(#14380,#14050);
#13831=PROPERTY_DEFINITION_REPRESENTATION(#14381,#14051);
#13832=PROPERTY_DEFINITION_REPRESENTATION(#14382,#14052);
#13833=PROPERTY_DEFINITION_REPRESENTATION(#14383,#14053);
#13834=PROPERTY_DEFINITION_REPRESENTATION(#14384,#14054);
#13835=PROPERTY_DEFINITION_REPRESENTATION(#14385,#14055);
#13836=PROPERTY_DEFINITION_REPRESENTATION(#14386,#14056);
#13837=PROPERTY_DEFINITION_REPRESENTATION(#14387,#14057);
#13838=PROPERTY_DEFINITION_REPRESENTATION(#14388,#14058);
#13839=PROPERTY_DEFINITION_REPRESENTATION(#14389,#14059);
#13840=PROPERTY_DEFINITION_REPRESENTATION(#14390,#14060);
#13841=PROPERTY_DEFINITION_REPRESENTATION(#14391,#14061);
#13842=PROPERTY_DEFINITION_REPRESENTATION(#14392,#14062);
#13843=PROPERTY_DEFINITION_REPRESENTATION(#14393,#14063);
#13844=PROPERTY_DEFINITION_REPRESENTATION(#14394,#14064);
#13845=PROPERTY_DEFINITION_REPRESENTATION(#14395,#14065);
#13846=PROPERTY_DEFINITION_REPRESENTATION(#14396,#14066);
#13847=PROPERTY_DEFINITION_REPRESENTATION(#14397,#14067);
#13848=PROPERTY_DEFINITION_REPRESENTATION(#14398,#14068);
#13849=PROPERTY_DEFINITION_REPRESENTATION(#14399,#14069);
#13850=PROPERTY_DEFINITION_REPRESENTATION(#14400,#14070);
#13851=PROPERTY_DEFINITION_REPRESENTATION(#14401,#14071);
#13852=PROPERTY_DEFINITION_REPRESENTATION(#14402,#14072);
#13853=PROPERTY_DEFINITION_REPRESENTATION(#14403,#14073);
#13854=PROPERTY_DEFINITION_REPRESENTATION(#14404,#14074);
#13855=PROPERTY_DEFINITION_REPRESENTATION(#14405,#14075);
#13856=PROPERTY_DEFINITION_REPRESENTATION(#14406,#14076);
#13857=PROPERTY_DEFINITION_REPRESENTATION(#14407,#14077);
#13858=PROPERTY_DEFINITION_REPRESENTATION(#14408,#14078);
#13859=PROPERTY_DEFINITION_REPRESENTATION(#14409,#14079);
#13860=PROPERTY_DEFINITION_REPRESENTATION(#14410,#14080);
#13861=PROPERTY_DEFINITION_REPRESENTATION(#14411,#14081);
#13862=PROPERTY_DEFINITION_REPRESENTATION(#14412,#14082);
#13863=PROPERTY_DEFINITION_REPRESENTATION(#14413,#14083);
#13864=PROPERTY_DEFINITION_REPRESENTATION(#14414,#14084);
#13865=PROPERTY_DEFINITION_REPRESENTATION(#14415,#14085);
#13866=PROPERTY_DEFINITION_REPRESENTATION(#14416,#14086);
#13867=PROPERTY_DEFINITION_REPRESENTATION(#14417,#14087);
#13868=PROPERTY_DEFINITION_REPRESENTATION(#14418,#14088);
#13869=PROPERTY_DEFINITION_REPRESENTATION(#14419,#14089);
#13870=PROPERTY_DEFINITION_REPRESENTATION(#14420,#14090);
#13871=PROPERTY_DEFINITION_REPRESENTATION(#14421,#14091);
#13872=PROPERTY_DEFINITION_REPRESENTATION(#14422,#14092);
#13873=PROPERTY_DEFINITION_REPRESENTATION(#14423,#14093);
#13874=PROPERTY_DEFINITION_REPRESENTATION(#14424,#14094);
#13875=PROPERTY_DEFINITION_REPRESENTATION(#14425,#14095);
#13876=PROPERTY_DEFINITION_REPRESENTATION(#14426,#14096);
#13877=PROPERTY_DEFINITION_REPRESENTATION(#14427,#14097);
#13878=PROPERTY_DEFINITION_REPRESENTATION(#14428,#14098);
#13879=PROPERTY_DEFINITION_REPRESENTATION(#14429,#14099);
#13880=PROPERTY_DEFINITION_REPRESENTATION(#14430,#14100);
#13881=PROPERTY_DEFINITION_REPRESENTATION(#14431,#14101);
#13882=PROPERTY_DEFINITION_REPRESENTATION(#14432,#14102);
#13883=PROPERTY_DEFINITION_REPRESENTATION(#14433,#14103);
#13884=PROPERTY_DEFINITION_REPRESENTATION(#14434,#14104);
#13885=PROPERTY_DEFINITION_REPRESENTATION(#14435,#14105);
#13886=PROPERTY_DEFINITION_REPRESENTATION(#14436,#14106);
#13887=PROPERTY_DEFINITION_REPRESENTATION(#14437,#14107);
#13888=PROPERTY_DEFINITION_REPRESENTATION(#14438,#14108);
#13889=PROPERTY_DEFINITION_REPRESENTATION(#14439,#14109);
#13890=PROPERTY_DEFINITION_REPRESENTATION(#14440,#14110);
#13891=PROPERTY_DEFINITION_REPRESENTATION(#14441,#14111);
#13892=PROPERTY_DEFINITION_REPRESENTATION(#14442,#14112);
#13893=PROPERTY_DEFINITION_REPRESENTATION(#14443,#14113);
#13894=PROPERTY_DEFINITION_REPRESENTATION(#14444,#14114);
#13895=PROPERTY_DEFINITION_REPRESENTATION(#14445,#14115);
#13896=PROPERTY_DEFINITION_REPRESENTATION(#14446,#14116);
#13897=PROPERTY_DEFINITION_REPRESENTATION(#14447,#14117);
#13898=PROPERTY_DEFINITION_REPRESENTATION(#14448,#14118);
#13899=PROPERTY_DEFINITION_REPRESENTATION(#14449,#14119);
#13900=PROPERTY_DEFINITION_REPRESENTATION(#14450,#14120);
#13901=PROPERTY_DEFINITION_REPRESENTATION(#14451,#14121);
#13902=PROPERTY_DEFINITION_REPRESENTATION(#14452,#14122);
#13903=PROPERTY_DEFINITION_REPRESENTATION(#14453,#14123);
#13904=PROPERTY_DEFINITION_REPRESENTATION(#14454,#14124);
#13905=PROPERTY_DEFINITION_REPRESENTATION(#14455,#14125);
#13906=PROPERTY_DEFINITION_REPRESENTATION(#14456,#14126);
#13907=PROPERTY_DEFINITION_REPRESENTATION(#14457,#14127);
#13908=PROPERTY_DEFINITION_REPRESENTATION(#14458,#14128);
#13909=PROPERTY_DEFINITION_REPRESENTATION(#14459,#14129);
#13910=PROPERTY_DEFINITION_REPRESENTATION(#14460,#14130);
#13911=PROPERTY_DEFINITION_REPRESENTATION(#14461,#14131);
#13912=PROPERTY_DEFINITION_REPRESENTATION(#14462,#14132);
#13913=PROPERTY_DEFINITION_REPRESENTATION(#14463,#14133);
#13914=PROPERTY_DEFINITION_REPRESENTATION(#14464,#14134);
#13915=PROPERTY_DEFINITION_REPRESENTATION(#14465,#14135);
#13916=PROPERTY_DEFINITION_REPRESENTATION(#14466,#14136);
#13917=PROPERTY_DEFINITION_REPRESENTATION(#14467,#14137);
#13918=PROPERTY_DEFINITION_REPRESENTATION(#14468,#14138);
#13919=PROPERTY_DEFINITION_REPRESENTATION(#14469,#14139);
#13920=PROPERTY_DEFINITION_REPRESENTATION(#14470,#14140);
#13921=PROPERTY_DEFINITION_REPRESENTATION(#14471,#14141);
#13922=PROPERTY_DEFINITION_REPRESENTATION(#14472,#14142);
#13923=PROPERTY_DEFINITION_REPRESENTATION(#14473,#14143);
#13924=PROPERTY_DEFINITION_REPRESENTATION(#14474,#14144);
#13925=PROPERTY_DEFINITION_REPRESENTATION(#14475,#14145);
#13926=PROPERTY_DEFINITION_REPRESENTATION(#14476,#14146);
#13927=PROPERTY_DEFINITION_REPRESENTATION(#14477,#14147);
#13928=PROPERTY_DEFINITION_REPRESENTATION(#14478,#14148);
#13929=PROPERTY_DEFINITION_REPRESENTATION(#14479,#14149);
#13930=PROPERTY_DEFINITION_REPRESENTATION(#14480,#14150);
#13931=PROPERTY_DEFINITION_REPRESENTATION(#14481,#14151);
#13932=PROPERTY_DEFINITION_REPRESENTATION(#14482,#14152);
#13933=PROPERTY_DEFINITION_REPRESENTATION(#14483,#14153);
#13934=PROPERTY_DEFINITION_REPRESENTATION(#14484,#14154);
#13935=PROPERTY_DEFINITION_REPRESENTATION(#14485,#14155);
#13936=PROPERTY_DEFINITION_REPRESENTATION(#14486,#14156);
#13937=PROPERTY_DEFINITION_REPRESENTATION(#14487,#14157);
#13938=PROPERTY_DEFINITION_REPRESENTATION(#14488,#14158);
#13939=PROPERTY_DEFINITION_REPRESENTATION(#14489,#14159);
#13940=PROPERTY_DEFINITION_REPRESENTATION(#14490,#14160);
#13941=PROPERTY_DEFINITION_REPRESENTATION(#14491,#14161);
#13942=PROPERTY_DEFINITION_REPRESENTATION(#14492,#14162);
#13943=PROPERTY_DEFINITION_REPRESENTATION(#14493,#14163);
#13944=PROPERTY_DEFINITION_REPRESENTATION(#14494,#14164);
#13945=PROPERTY_DEFINITION_REPRESENTATION(#14495,#14165);
#13946=PROPERTY_DEFINITION_REPRESENTATION(#14496,#14166);
#13947=PROPERTY_DEFINITION_REPRESENTATION(#14497,#14167);
#13948=PROPERTY_DEFINITION_REPRESENTATION(#14498,#14168);
#13949=PROPERTY_DEFINITION_REPRESENTATION(#14499,#14169);
#13950=PROPERTY_DEFINITION_REPRESENTATION(#14500,#14170);
#13951=PROPERTY_DEFINITION_REPRESENTATION(#14501,#14171);
#13952=PROPERTY_DEFINITION_REPRESENTATION(#14502,#14172);
#13953=PROPERTY_DEFINITION_REPRESENTATION(#14503,#14173);
#13954=PROPERTY_DEFINITION_REPRESENTATION(#14504,#14174);
#13955=PROPERTY_DEFINITION_REPRESENTATION(#14505,#14175);
#13956=PROPERTY_DEFINITION_REPRESENTATION(#14506,#14176);
#13957=PROPERTY_DEFINITION_REPRESENTATION(#14507,#14177);
#13958=PROPERTY_DEFINITION_REPRESENTATION(#14508,#14178);
#13959=PROPERTY_DEFINITION_REPRESENTATION(#14509,#14179);
#13960=PROPERTY_DEFINITION_REPRESENTATION(#14510,#14180);
#13961=PROPERTY_DEFINITION_REPRESENTATION(#14511,#14181);
#13962=PROPERTY_DEFINITION_REPRESENTATION(#14512,#14182);
#13963=PROPERTY_DEFINITION_REPRESENTATION(#14513,#14183);
#13964=PROPERTY_DEFINITION_REPRESENTATION(#14514,#14184);
#13965=PROPERTY_DEFINITION_REPRESENTATION(#14515,#14185);
#13966=PROPERTY_DEFINITION_REPRESENTATION(#14516,#14186);
#13967=PROPERTY_DEFINITION_REPRESENTATION(#14517,#14187);
#13968=PROPERTY_DEFINITION_REPRESENTATION(#14518,#14188);
#13969=PROPERTY_DEFINITION_REPRESENTATION(#14519,#14189);
#13970=PROPERTY_DEFINITION_REPRESENTATION(#14520,#14190);
#13971=PROPERTY_DEFINITION_REPRESENTATION(#14521,#14191);
#13972=PROPERTY_DEFINITION_REPRESENTATION(#14522,#14192);
#13973=PROPERTY_DEFINITION_REPRESENTATION(#14523,#14193);
#13974=PROPERTY_DEFINITION_REPRESENTATION(#14524,#14194);
#13975=PROPERTY_DEFINITION_REPRESENTATION(#14525,#14195);
#13976=PROPERTY_DEFINITION_REPRESENTATION(#14526,#14196);
#13977=PROPERTY_DEFINITION_REPRESENTATION(#14527,#14197);
#13978=PROPERTY_DEFINITION_REPRESENTATION(#14528,#14198);
#13979=PROPERTY_DEFINITION_REPRESENTATION(#14529,#14199);
#13980=PROPERTY_DEFINITION_REPRESENTATION(#14530,#14200);
#13981=PROPERTY_DEFINITION_REPRESENTATION(#14531,#14201);
#13982=PROPERTY_DEFINITION_REPRESENTATION(#14532,#14202);
#13983=PROPERTY_DEFINITION_REPRESENTATION(#14533,#14203);
#13984=PROPERTY_DEFINITION_REPRESENTATION(#14534,#14204);
#13985=PROPERTY_DEFINITION_REPRESENTATION(#14535,#14205);
#13986=PROPERTY_DEFINITION_REPRESENTATION(#14536,#14206);
#13987=PROPERTY_DEFINITION_REPRESENTATION(#14537,#14207);
#13988=PROPERTY_DEFINITION_REPRESENTATION(#14538,#14208);
#13989=PROPERTY_DEFINITION_REPRESENTATION(#14539,#14209);
#13990=PROPERTY_DEFINITION_REPRESENTATION(#14540,#14210);
#13991=PROPERTY_DEFINITION_REPRESENTATION(#14541,#14211);
#13992=PROPERTY_DEFINITION_REPRESENTATION(#14542,#14212);
#13993=PROPERTY_DEFINITION_REPRESENTATION(#14543,#14213);
#13994=PROPERTY_DEFINITION_REPRESENTATION(#14544,#14214);
#13995=PROPERTY_DEFINITION_REPRESENTATION(#14545,#14215);
#13996=PROPERTY_DEFINITION_REPRESENTATION(#14546,#14216);
#13997=PROPERTY_DEFINITION_REPRESENTATION(#14547,#14217);
#13998=PROPERTY_DEFINITION_REPRESENTATION(#14548,#14218);
#13999=PROPERTY_DEFINITION_REPRESENTATION(#14549,#14219);
#14000=PROPERTY_DEFINITION_REPRESENTATION(#14550,#14220);
#14001=PROPERTY_DEFINITION_REPRESENTATION(#14551,#14221);
#14002=PROPERTY_DEFINITION_REPRESENTATION(#14552,#14222);
#14003=PROPERTY_DEFINITION_REPRESENTATION(#14553,#14223);
#14004=PROPERTY_DEFINITION_REPRESENTATION(#14554,#14224);
#14005=PROPERTY_DEFINITION_REPRESENTATION(#14555,#14225);
#14006=PROPERTY_DEFINITION_REPRESENTATION(#14556,#14226);
#14007=PROPERTY_DEFINITION_REPRESENTATION(#14557,#14227);
#14008=PROPERTY_DEFINITION_REPRESENTATION(#14558,#14228);
#14009=PROPERTY_DEFINITION_REPRESENTATION(#14559,#14229);
#14010=PROPERTY_DEFINITION_REPRESENTATION(#14560,#14230);
#14011=PROPERTY_DEFINITION_REPRESENTATION(#14561,#14231);
#14012=PROPERTY_DEFINITION_REPRESENTATION(#14562,#14232);
#14013=PROPERTY_DEFINITION_REPRESENTATION(#14563,#14233);
#14014=PROPERTY_DEFINITION_REPRESENTATION(#14564,#14234);
#14015=PROPERTY_DEFINITION_REPRESENTATION(#14565,#14235);
#14016=PROPERTY_DEFINITION_REPRESENTATION(#14566,#14236);
#14017=PROPERTY_DEFINITION_REPRESENTATION(#14567,#14237);
#14018=PROPERTY_DEFINITION_REPRESENTATION(#14568,#14238);
#14019=PROPERTY_DEFINITION_REPRESENTATION(#14569,#14239);
#14020=PROPERTY_DEFINITION_REPRESENTATION(#14570,#14240);
#14021=PROPERTY_DEFINITION_REPRESENTATION(#14571,#14241);
#14022=PROPERTY_DEFINITION_REPRESENTATION(#14572,#14242);
#14023=PROPERTY_DEFINITION_REPRESENTATION(#14573,#14243);
#14024=PROPERTY_DEFINITION_REPRESENTATION(#14574,#14244);
#14025=PROPERTY_DEFINITION_REPRESENTATION(#14575,#14245);
#14026=PROPERTY_DEFINITION_REPRESENTATION(#14576,#14246);
#14027=PROPERTY_DEFINITION_REPRESENTATION(#14577,#14247);
#14028=PROPERTY_DEFINITION_REPRESENTATION(#14578,#14248);
#14029=PROPERTY_DEFINITION_REPRESENTATION(#14579,#14249);
#14030=PROPERTY_DEFINITION_REPRESENTATION(#14580,#14250);
#14031=PROPERTY_DEFINITION_REPRESENTATION(#14581,#14251);
#14032=PROPERTY_DEFINITION_REPRESENTATION(#14582,#14252);
#14033=PROPERTY_DEFINITION_REPRESENTATION(#14583,#14253);
#14034=PROPERTY_DEFINITION_REPRESENTATION(#14584,#14254);
#14035=REPRESENTATION('material name',(#14255),#24982);
#14036=REPRESENTATION('density',(#13705),#24982);
#14037=REPRESENTATION('material name',(#14256),#24983);
#14038=REPRESENTATION('density',(#13706),#24983);
#14039=REPRESENTATION('material name',(#14257),#24984);
#14040=REPRESENTATION('density',(#13707),#24984);
#14041=REPRESENTATION('material name',(#14258),#24985);
#14042=REPRESENTATION('density',(#13708),#24985);
#14043=REPRESENTATION('material name',(#14259),#24986);
#14044=REPRESENTATION('density',(#13709),#24986);
#14045=REPRESENTATION('material name',(#14260),#24987);
#14046=REPRESENTATION('density',(#13710),#24987);
#14047=REPRESENTATION('material name',(#14261),#24988);
#14048=REPRESENTATION('density',(#13711),#24988);
#14049=REPRESENTATION('material name',(#14262),#24989);
#14050=REPRESENTATION('density',(#13712),#24989);
#14051=REPRESENTATION('material name',(#14263),#24990);
#14052=REPRESENTATION('density',(#13713),#24990);
#14053=REPRESENTATION('material name',(#14264),#24991);
#14054=REPRESENTATION('density',(#13714),#24991);
#14055=REPRESENTATION('material name',(#14265),#24992);
#14056=REPRESENTATION('density',(#13715),#24992);
#14057=REPRESENTATION('material name',(#14266),#24993);
#14058=REPRESENTATION('density',(#13716),#24993);
#14059=REPRESENTATION('material name',(#14267),#24994);
#14060=REPRESENTATION('density',(#13717),#24994);
#14061=REPRESENTATION('material name',(#14268),#24995);
#14062=REPRESENTATION('density',(#13718),#24995);
#14063=REPRESENTATION('material name',(#14269),#24996);
#14064=REPRESENTATION('density',(#13719),#24996);
#14065=REPRESENTATION('material name',(#14270),#24997);
#14066=REPRESENTATION('density',(#13720),#24997);
#14067=REPRESENTATION('material name',(#14271),#24998);
#14068=REPRESENTATION('density',(#13721),#24998);
#14069=REPRESENTATION('material name',(#14272),#24999);
#14070=REPRESENTATION('density',(#13722),#24999);
#14071=REPRESENTATION('material name',(#14273),#25001);
#14072=REPRESENTATION('density',(#13723),#25001);
#14073=REPRESENTATION('material name',(#14274),#25002);
#14074=REPRESENTATION('density',(#13724),#25002);
#14075=REPRESENTATION('material name',(#14275),#25003);
#14076=REPRESENTATION('density',(#13725),#25003);
#14077=REPRESENTATION('material name',(#14276),#25004);
#14078=REPRESENTATION('density',(#13726),#25004);
#14079=REPRESENTATION('material name',(#14277),#25005);
#14080=REPRESENTATION('density',(#13727),#25005);
#14081=REPRESENTATION('material name',(#14278),#25006);
#14082=REPRESENTATION('density',(#13728),#25006);
#14083=REPRESENTATION('material name',(#14279),#25007);
#14084=REPRESENTATION('density',(#13729),#25007);
#14085=REPRESENTATION('material name',(#14280),#25008);
#14086=REPRESENTATION('density',(#13730),#25008);
#14087=REPRESENTATION('material name',(#14281),#25009);
#14088=REPRESENTATION('density',(#13731),#25009);
#14089=REPRESENTATION('material name',(#14282),#25010);
#14090=REPRESENTATION('density',(#13732),#25010);
#14091=REPRESENTATION('material name',(#14283),#25011);
#14092=REPRESENTATION('density',(#13733),#25011);
#14093=REPRESENTATION('material name',(#14284),#25012);
#14094=REPRESENTATION('density',(#13734),#25012);
#14095=REPRESENTATION('material name',(#14285),#25013);
#14096=REPRESENTATION('density',(#13735),#25013);
#14097=REPRESENTATION('material name',(#14286),#25015);
#14098=REPRESENTATION('density',(#13736),#25015);
#14099=REPRESENTATION('material name',(#14287),#25016);
#14100=REPRESENTATION('density',(#13737),#25016);
#14101=REPRESENTATION('material name',(#14288),#25017);
#14102=REPRESENTATION('density',(#13738),#25017);
#14103=REPRESENTATION('material name',(#14289),#25018);
#14104=REPRESENTATION('density',(#13739),#25018);
#14105=REPRESENTATION('material name',(#14290),#25019);
#14106=REPRESENTATION('density',(#13740),#25019);
#14107=REPRESENTATION('material name',(#14291),#25020);
#14108=REPRESENTATION('density',(#13741),#25020);
#14109=REPRESENTATION('material name',(#14292),#25021);
#14110=REPRESENTATION('density',(#13742),#25021);
#14111=REPRESENTATION('material name',(#14293),#25022);
#14112=REPRESENTATION('density',(#13743),#25022);
#14113=REPRESENTATION('material name',(#14294),#25023);
#14114=REPRESENTATION('density',(#13744),#25023);
#14115=REPRESENTATION('material name',(#14295),#25024);
#14116=REPRESENTATION('density',(#13745),#25024);
#14117=REPRESENTATION('material name',(#14296),#25025);
#14118=REPRESENTATION('density',(#13746),#25025);
#14119=REPRESENTATION('material name',(#14297),#25027);
#14120=REPRESENTATION('density',(#13747),#25027);
#14121=REPRESENTATION('material name',(#14298),#25028);
#14122=REPRESENTATION('density',(#13748),#25028);
#14123=REPRESENTATION('material name',(#14299),#25029);
#14124=REPRESENTATION('density',(#13749),#25029);
#14125=REPRESENTATION('material name',(#14300),#25030);
#14126=REPRESENTATION('density',(#13750),#25030);
#14127=REPRESENTATION('material name',(#14301),#25031);
#14128=REPRESENTATION('density',(#13751),#25031);
#14129=REPRESENTATION('material name',(#14302),#25032);
#14130=REPRESENTATION('density',(#13752),#25032);
#14131=REPRESENTATION('material name',(#14303),#25033);
#14132=REPRESENTATION('density',(#13753),#25033);
#14133=REPRESENTATION('material name',(#14304),#25034);
#14134=REPRESENTATION('density',(#13754),#25034);
#14135=REPRESENTATION('material name',(#14305),#25035);
#14136=REPRESENTATION('density',(#13755),#25035);
#14137=REPRESENTATION('material name',(#14306),#25036);
#14138=REPRESENTATION('density',(#13756),#25036);
#14139=REPRESENTATION('material name',(#14307),#25037);
#14140=REPRESENTATION('density',(#13757),#25037);
#14141=REPRESENTATION('material name',(#14308),#25039);
#14142=REPRESENTATION('density',(#13758),#25039);
#14143=REPRESENTATION('material name',(#14309),#25040);
#14144=REPRESENTATION('density',(#13759),#25040);
#14145=REPRESENTATION('material name',(#14310),#25041);
#14146=REPRESENTATION('density',(#13760),#25041);
#14147=REPRESENTATION('material name',(#14311),#25043);
#14148=REPRESENTATION('density',(#13761),#25043);
#14149=REPRESENTATION('material name',(#14312),#25044);
#14150=REPRESENTATION('density',(#13762),#25044);
#14151=REPRESENTATION('material name',(#14313),#25045);
#14152=REPRESENTATION('density',(#13763),#25045);
#14153=REPRESENTATION('material name',(#14314),#25046);
#14154=REPRESENTATION('density',(#13764),#25046);
#14155=REPRESENTATION('material name',(#14315),#25047);
#14156=REPRESENTATION('density',(#13765),#25047);
#14157=REPRESENTATION('material name',(#14316),#25048);
#14158=REPRESENTATION('density',(#13766),#25048);
#14159=REPRESENTATION('material name',(#14317),#25049);
#14160=REPRESENTATION('density',(#13767),#25049);
#14161=REPRESENTATION('material name',(#14318),#25050);
#14162=REPRESENTATION('density',(#13768),#25050);
#14163=REPRESENTATION('material name',(#14319),#25051);
#14164=REPRESENTATION('density',(#13769),#25051);
#14165=REPRESENTATION('material name',(#14320),#25052);
#14166=REPRESENTATION('density',(#13770),#25052);
#14167=REPRESENTATION('material name',(#14321),#25053);
#14168=REPRESENTATION('density',(#13771),#25053);
#14169=REPRESENTATION('material name',(#14322),#25054);
#14170=REPRESENTATION('density',(#13772),#25054);
#14171=REPRESENTATION('material name',(#14323),#25055);
#14172=REPRESENTATION('density',(#13773),#25055);
#14173=REPRESENTATION('material name',(#14324),#25056);
#14174=REPRESENTATION('density',(#13774),#25056);
#14175=REPRESENTATION('material name',(#14325),#25057);
#14176=REPRESENTATION('density',(#13775),#25057);
#14177=REPRESENTATION('material name',(#14326),#25058);
#14178=REPRESENTATION('density',(#13776),#25058);
#14179=REPRESENTATION('material name',(#14327),#25059);
#14180=REPRESENTATION('density',(#13777),#25059);
#14181=REPRESENTATION('material name',(#14328),#25061);
#14182=REPRESENTATION('density',(#13778),#25061);
#14183=REPRESENTATION('material name',(#14329),#25062);
#14184=REPRESENTATION('density',(#13779),#25062);
#14185=REPRESENTATION('material name',(#14330),#25063);
#14186=REPRESENTATION('density',(#13780),#25063);
#14187=REPRESENTATION('material name',(#14331),#25064);
#14188=REPRESENTATION('density',(#13781),#25064);
#14189=REPRESENTATION('material name',(#14332),#25065);
#14190=REPRESENTATION('density',(#13782),#25065);
#14191=REPRESENTATION('material name',(#14333),#25066);
#14192=REPRESENTATION('density',(#13783),#25066);
#14193=REPRESENTATION('material name',(#14334),#25067);
#14194=REPRESENTATION('density',(#13784),#25067);
#14195=REPRESENTATION('material name',(#14335),#25068);
#14196=REPRESENTATION('density',(#13785),#25068);
#14197=REPRESENTATION('material name',(#14336),#25069);
#14198=REPRESENTATION('density',(#13786),#25069);
#14199=REPRESENTATION('material name',(#14337),#25070);
#14200=REPRESENTATION('density',(#13787),#25070);
#14201=REPRESENTATION('material name',(#14338),#25071);
#14202=REPRESENTATION('density',(#13788),#25071);
#14203=REPRESENTATION('material name',(#14339),#25072);
#14204=REPRESENTATION('density',(#13789),#25072);
#14205=REPRESENTATION('material name',(#14340),#25073);
#14206=REPRESENTATION('density',(#13790),#25073);
#14207=REPRESENTATION('material name',(#14341),#25074);
#14208=REPRESENTATION('density',(#13791),#25074);
#14209=REPRESENTATION('material name',(#14342),#25075);
#14210=REPRESENTATION('density',(#13792),#25075);
#14211=REPRESENTATION('material name',(#14343),#25076);
#14212=REPRESENTATION('density',(#13793),#25076);
#14213=REPRESENTATION('material name',(#14344),#25077);
#14214=REPRESENTATION('density',(#13794),#25077);
#14215=REPRESENTATION('material name',(#14345),#25078);
#14216=REPRESENTATION('density',(#13795),#25078);
#14217=REPRESENTATION('material name',(#14346),#25079);
#14218=REPRESENTATION('density',(#13796),#25079);
#14219=REPRESENTATION('material name',(#14347),#25080);
#14220=REPRESENTATION('density',(#13797),#25080);
#14221=REPRESENTATION('material name',(#14348),#25081);
#14222=REPRESENTATION('density',(#13798),#25081);
#14223=REPRESENTATION('material name',(#14349),#25082);
#14224=REPRESENTATION('density',(#13799),#25082);
#14225=REPRESENTATION('material name',(#14350),#25083);
#14226=REPRESENTATION('density',(#13800),#25083);
#14227=REPRESENTATION('material name',(#14351),#25084);
#14228=REPRESENTATION('density',(#13801),#25084);
#14229=REPRESENTATION('material name',(#14352),#25085);
#14230=REPRESENTATION('density',(#13802),#25085);
#14231=REPRESENTATION('material name',(#14353),#25086);
#14232=REPRESENTATION('density',(#13803),#25086);
#14233=REPRESENTATION('material name',(#14354),#25088);
#14234=REPRESENTATION('density',(#13804),#25088);
#14235=REPRESENTATION('material name',(#14355),#25089);
#14236=REPRESENTATION('density',(#13805),#25089);
#14237=REPRESENTATION('material name',(#14356),#25090);
#14238=REPRESENTATION('density',(#13806),#25090);
#14239=REPRESENTATION('material name',(#14357),#25091);
#14240=REPRESENTATION('density',(#13807),#25091);
#14241=REPRESENTATION('material name',(#14358),#25092);
#14242=REPRESENTATION('density',(#13808),#25092);
#14243=REPRESENTATION('material name',(#14359),#25094);
#14244=REPRESENTATION('density',(#13809),#25094);
#14245=REPRESENTATION('material name',(#14360),#25095);
#14246=REPRESENTATION('density',(#13810),#25095);
#14247=REPRESENTATION('material name',(#14361),#25096);
#14248=REPRESENTATION('density',(#13811),#25096);
#14249=REPRESENTATION('material name',(#14362),#25097);
#14250=REPRESENTATION('density',(#13812),#25097);
#14251=REPRESENTATION('material name',(#14363),#25098);
#14252=REPRESENTATION('density',(#13813),#25098);
#14253=REPRESENTATION('material name',(#14364),#25099);
#14254=REPRESENTATION('density',(#13814),#25099);
#14255=DESCRIPTIVE_REPRESENTATION_ITEM('Steel','Steel');
#14256=DESCRIPTIVE_REPRESENTATION_ITEM('Steel','Steel');
#14257=DESCRIPTIVE_REPRESENTATION_ITEM('Steel','Steel');
#14258=DESCRIPTIVE_REPRESENTATION_ITEM('Steel','Steel');
#14259=DESCRIPTIVE_REPRESENTATION_ITEM('Steel','Steel');
#14260=DESCRIPTIVE_REPRESENTATION_ITEM('Steel','Steel');
#14261=DESCRIPTIVE_REPRESENTATION_ITEM('Steel','Steel');
#14262=DESCRIPTIVE_REPRESENTATION_ITEM('Steel','Steel');
#14263=DESCRIPTIVE_REPRESENTATION_ITEM('Steel','Steel');
#14264=DESCRIPTIVE_REPRESENTATION_ITEM('Steel','Steel');
#14265=DESCRIPTIVE_REPRESENTATION_ITEM('Steel','Steel');
#14266=DESCRIPTIVE_REPRESENTATION_ITEM('Steel','Steel');
#14267=DESCRIPTIVE_REPRESENTATION_ITEM('Steel','Steel');
#14268=DESCRIPTIVE_REPRESENTATION_ITEM('Steel','Steel');
#14269=DESCRIPTIVE_REPRESENTATION_ITEM('Steel','Steel');
#14270=DESCRIPTIVE_REPRESENTATION_ITEM('Steel','Steel');
#14271=DESCRIPTIVE_REPRESENTATION_ITEM('Steel','Steel');
#14272=DESCRIPTIVE_REPRESENTATION_ITEM('Steel','Steel');
#14273=DESCRIPTIVE_REPRESENTATION_ITEM('Steel','Steel');
#14274=DESCRIPTIVE_REPRESENTATION_ITEM('Steel','Steel');
#14275=DESCRIPTIVE_REPRESENTATION_ITEM('Steel','Steel');
#14276=DESCRIPTIVE_REPRESENTATION_ITEM('Steel','Steel');
#14277=DESCRIPTIVE_REPRESENTATION_ITEM('Steel','Steel');
#14278=DESCRIPTIVE_REPRESENTATION_ITEM('Steel','Steel');
#14279=DESCRIPTIVE_REPRESENTATION_ITEM('Steel','Steel');
#14280=DESCRIPTIVE_REPRESENTATION_ITEM('Steel','Steel');
#14281=DESCRIPTIVE_REPRESENTATION_ITEM('Steel','Steel');
#14282=DESCRIPTIVE_REPRESENTATION_ITEM('Steel','Steel');
#14283=DESCRIPTIVE_REPRESENTATION_ITEM('Steel','Steel');
#14284=DESCRIPTIVE_REPRESENTATION_ITEM('Steel','Steel');
#14285=DESCRIPTIVE_REPRESENTATION_ITEM('Steel','Steel');
#14286=DESCRIPTIVE_REPRESENTATION_ITEM('Steel','Steel');
#14287=DESCRIPTIVE_REPRESENTATION_ITEM('Steel','Steel');
#14288=DESCRIPTIVE_REPRESENTATION_ITEM('Steel','Steel');
#14289=DESCRIPTIVE_REPRESENTATION_ITEM('Steel','Steel');
#14290=DESCRIPTIVE_REPRESENTATION_ITEM('Steel','Steel');
#14291=DESCRIPTIVE_REPRESENTATION_ITEM('Steel','Steel');
#14292=DESCRIPTIVE_REPRESENTATION_ITEM('Steel','Steel');
#14293=DESCRIPTIVE_REPRESENTATION_ITEM('Steel','Steel');
#14294=DESCRIPTIVE_REPRESENTATION_ITEM('Steel','Steel');
#14295=DESCRIPTIVE_REPRESENTATION_ITEM('Steel','Steel');
#14296=DESCRIPTIVE_REPRESENTATION_ITEM('Steel','Steel');
#14297=DESCRIPTIVE_REPRESENTATION_ITEM('Steel','Steel');
#14298=DESCRIPTIVE_REPRESENTATION_ITEM('Steel','Steel');
#14299=DESCRIPTIVE_REPRESENTATION_ITEM('Steel','Steel');
#14300=DESCRIPTIVE_REPRESENTATION_ITEM('Steel','Steel');
#14301=DESCRIPTIVE_REPRESENTATION_ITEM('Steel','Steel');
#14302=DESCRIPTIVE_REPRESENTATION_ITEM('Steel','Steel');
#14303=DESCRIPTIVE_REPRESENTATION_ITEM('Steel','Steel');
#14304=DESCRIPTIVE_REPRESENTATION_ITEM('Steel','Steel');
#14305=DESCRIPTIVE_REPRESENTATION_ITEM('Steel','Steel');
#14306=DESCRIPTIVE_REPRESENTATION_ITEM('Steel','Steel');
#14307=DESCRIPTIVE_REPRESENTATION_ITEM('Steel','Steel');
#14308=DESCRIPTIVE_REPRESENTATION_ITEM('Steel','Steel');
#14309=DESCRIPTIVE_REPRESENTATION_ITEM('Steel','Steel');
#14310=DESCRIPTIVE_REPRESENTATION_ITEM('Steel','Steel');
#14311=DESCRIPTIVE_REPRESENTATION_ITEM('Steel','Steel');
#14312=DESCRIPTIVE_REPRESENTATION_ITEM('Steel','Steel');
#14313=DESCRIPTIVE_REPRESENTATION_ITEM('Steel','Steel');
#14314=DESCRIPTIVE_REPRESENTATION_ITEM('Steel','Steel');
#14315=DESCRIPTIVE_REPRESENTATION_ITEM('Steel','Steel');
#14316=DESCRIPTIVE_REPRESENTATION_ITEM('Steel','Steel');
#14317=DESCRIPTIVE_REPRESENTATION_ITEM('Steel','Steel');
#14318=DESCRIPTIVE_REPRESENTATION_ITEM('Steel','Steel');
#14319=DESCRIPTIVE_REPRESENTATION_ITEM('Steel','Steel');
#14320=DESCRIPTIVE_REPRESENTATION_ITEM('Steel','Steel');
#14321=DESCRIPTIVE_REPRESENTATION_ITEM('Steel','Steel');
#14322=DESCRIPTIVE_REPRESENTATION_ITEM('Steel','Steel');
#14323=DESCRIPTIVE_REPRESENTATION_ITEM('Steel','Steel');
#14324=DESCRIPTIVE_REPRESENTATION_ITEM('Steel','Steel');
#14325=DESCRIPTIVE_REPRESENTATION_ITEM('Steel','Steel');
#14326=DESCRIPTIVE_REPRESENTATION_ITEM('Steel','Steel');
#14327=DESCRIPTIVE_REPRESENTATION_ITEM('Steel','Steel');
#14328=DESCRIPTIVE_REPRESENTATION_ITEM('Steel','Steel');
#14329=DESCRIPTIVE_REPRESENTATION_ITEM('Steel','Steel');
#14330=DESCRIPTIVE_REPRESENTATION_ITEM('Steel','Steel');
#14331=DESCRIPTIVE_REPRESENTATION_ITEM('Steel','Steel');
#14332=DESCRIPTIVE_REPRESENTATION_ITEM('Steel','Steel');
#14333=DESCRIPTIVE_REPRESENTATION_ITEM('Steel','Steel');
#14334=DESCRIPTIVE_REPRESENTATION_ITEM('Steel','Steel');
#14335=DESCRIPTIVE_REPRESENTATION_ITEM('Steel','Steel');
#14336=DESCRIPTIVE_REPRESENTATION_ITEM('Steel','Steel');
#14337=DESCRIPTIVE_REPRESENTATION_ITEM('Steel','Steel');
#14338=DESCRIPTIVE_REPRESENTATION_ITEM('Steel','Steel');
#14339=DESCRIPTIVE_REPRESENTATION_ITEM('Steel','Steel');
#14340=DESCRIPTIVE_REPRESENTATION_ITEM('Steel','Steel');
#14341=DESCRIPTIVE_REPRESENTATION_ITEM('Steel','Steel');
#14342=DESCRIPTIVE_REPRESENTATION_ITEM('Steel','Steel');
#14343=DESCRIPTIVE_REPRESENTATION_ITEM('Steel','Steel');
#14344=DESCRIPTIVE_REPRESENTATION_ITEM('Steel','Steel');
#14345=DESCRIPTIVE_REPRESENTATION_ITEM('Steel','Steel');
#14346=DESCRIPTIVE_REPRESENTATION_ITEM('Steel','Steel');
#14347=DESCRIPTIVE_REPRESENTATION_ITEM('Steel','Steel');
#14348=DESCRIPTIVE_REPRESENTATION_ITEM('Steel','Steel');
#14349=DESCRIPTIVE_REPRESENTATION_ITEM('Steel','Steel');
#14350=DESCRIPTIVE_REPRESENTATION_ITEM('Steel','Steel');
#14351=DESCRIPTIVE_REPRESENTATION_ITEM('Steel','Steel');
#14352=DESCRIPTIVE_REPRESENTATION_ITEM('Steel','Steel');
#14353=DESCRIPTIVE_REPRESENTATION_ITEM('Steel','Steel');
#14354=DESCRIPTIVE_REPRESENTATION_ITEM('Steel','Steel');
#14355=DESCRIPTIVE_REPRESENTATION_ITEM('Steel','Steel');
#14356=DESCRIPTIVE_REPRESENTATION_ITEM('Steel','Steel');
#14357=DESCRIPTIVE_REPRESENTATION_ITEM('Steel','Steel');
#14358=DESCRIPTIVE_REPRESENTATION_ITEM('Steel','Steel');
#14359=DESCRIPTIVE_REPRESENTATION_ITEM('Steel','Steel');
#14360=DESCRIPTIVE_REPRESENTATION_ITEM('Steel','Steel');
#14361=DESCRIPTIVE_REPRESENTATION_ITEM('Steel','Steel');
#14362=DESCRIPTIVE_REPRESENTATION_ITEM('Steel','Steel');
#14363=DESCRIPTIVE_REPRESENTATION_ITEM('Steel','Steel');
#14364=DESCRIPTIVE_REPRESENTATION_ITEM('Steel','Steel');
#14365=PROPERTY_DEFINITION('material property','material name',#25633);
#14366=PROPERTY_DEFINITION('material property','density of part',#25633);
#14367=PROPERTY_DEFINITION('material property','material name',#25634);
#14368=PROPERTY_DEFINITION('material property','density of part',#25634);
#14369=PROPERTY_DEFINITION('material property','material name',#25635);
#14370=PROPERTY_DEFINITION('material property','density of part',#25635);
#14371=PROPERTY_DEFINITION('material property','material name',#25636);
#14372=PROPERTY_DEFINITION('material property','density of part',#25636);
#14373=PROPERTY_DEFINITION('material property','material name',#25637);
#14374=PROPERTY_DEFINITION('material property','density of part',#25637);
#14375=PROPERTY_DEFINITION('material property','material name',#25638);
#14376=PROPERTY_DEFINITION('material property','density of part',#25638);
#14377=PROPERTY_DEFINITION('material property','material name',#25639);
#14378=PROPERTY_DEFINITION('material property','density of part',#25639);
#14379=PROPERTY_DEFINITION('material property','material name',#25640);
#14380=PROPERTY_DEFINITION('material property','density of part',#25640);
#14381=PROPERTY_DEFINITION('material property','material name',#25641);
#14382=PROPERTY_DEFINITION('material property','density of part',#25641);
#14383=PROPERTY_DEFINITION('material property','material name',#25642);
#14384=PROPERTY_DEFINITION('material property','density of part',#25642);
#14385=PROPERTY_DEFINITION('material property','material name',#25643);
#14386=PROPERTY_DEFINITION('material property','density of part',#25643);
#14387=PROPERTY_DEFINITION('material property','material name',#25644);
#14388=PROPERTY_DEFINITION('material property','density of part',#25644);
#14389=PROPERTY_DEFINITION('material property','material name',#25645);
#14390=PROPERTY_DEFINITION('material property','density of part',#25645);
#14391=PROPERTY_DEFINITION('material property','material name',#25646);
#14392=PROPERTY_DEFINITION('material property','density of part',#25646);
#14393=PROPERTY_DEFINITION('material property','material name',#25647);
#14394=PROPERTY_DEFINITION('material property','density of part',#25647);
#14395=PROPERTY_DEFINITION('material property','material name',#25648);
#14396=PROPERTY_DEFINITION('material property','density of part',#25648);
#14397=PROPERTY_DEFINITION('material property','material name',#25649);
#14398=PROPERTY_DEFINITION('material property','density of part',#25649);
#14399=PROPERTY_DEFINITION('material property','material name',#25650);
#14400=PROPERTY_DEFINITION('material property','density of part',#25650);
#14401=PROPERTY_DEFINITION('material property','material name',#25652);
#14402=PROPERTY_DEFINITION('material property','density of part',#25652);
#14403=PROPERTY_DEFINITION('material property','material name',#25653);
#14404=PROPERTY_DEFINITION('material property','density of part',#25653);
#14405=PROPERTY_DEFINITION('material property','material name',#25654);
#14406=PROPERTY_DEFINITION('material property','density of part',#25654);
#14407=PROPERTY_DEFINITION('material property','material name',#25655);
#14408=PROPERTY_DEFINITION('material property','density of part',#25655);
#14409=PROPERTY_DEFINITION('material property','material name',#25656);
#14410=PROPERTY_DEFINITION('material property','density of part',#25656);
#14411=PROPERTY_DEFINITION('material property','material name',#25657);
#14412=PROPERTY_DEFINITION('material property','density of part',#25657);
#14413=PROPERTY_DEFINITION('material property','material name',#25658);
#14414=PROPERTY_DEFINITION('material property','density of part',#25658);
#14415=PROPERTY_DEFINITION('material property','material name',#25659);
#14416=PROPERTY_DEFINITION('material property','density of part',#25659);
#14417=PROPERTY_DEFINITION('material property','material name',#25660);
#14418=PROPERTY_DEFINITION('material property','density of part',#25660);
#14419=PROPERTY_DEFINITION('material property','material name',#25661);
#14420=PROPERTY_DEFINITION('material property','density of part',#25661);
#14421=PROPERTY_DEFINITION('material property','material name',#25662);
#14422=PROPERTY_DEFINITION('material property','density of part',#25662);
#14423=PROPERTY_DEFINITION('material property','material name',#25663);
#14424=PROPERTY_DEFINITION('material property','density of part',#25663);
#14425=PROPERTY_DEFINITION('material property','material name',#25664);
#14426=PROPERTY_DEFINITION('material property','density of part',#25664);
#14427=PROPERTY_DEFINITION('material property','material name',#25666);
#14428=PROPERTY_DEFINITION('material property','density of part',#25666);
#14429=PROPERTY_DEFINITION('material property','material name',#25667);
#14430=PROPERTY_DEFINITION('material property','density of part',#25667);
#14431=PROPERTY_DEFINITION('material property','material name',#25668);
#14432=PROPERTY_DEFINITION('material property','density of part',#25668);
#14433=PROPERTY_DEFINITION('material property','material name',#25669);
#14434=PROPERTY_DEFINITION('material property','density of part',#25669);
#14435=PROPERTY_DEFINITION('material property','material name',#25670);
#14436=PROPERTY_DEFINITION('material property','density of part',#25670);
#14437=PROPERTY_DEFINITION('material property','material name',#25671);
#14438=PROPERTY_DEFINITION('material property','density of part',#25671);
#14439=PROPERTY_DEFINITION('material property','material name',#25672);
#14440=PROPERTY_DEFINITION('material property','density of part',#25672);
#14441=PROPERTY_DEFINITION('material property','material name',#25673);
#14442=PROPERTY_DEFINITION('material property','density of part',#25673);
#14443=PROPERTY_DEFINITION('material property','material name',#25674);
#14444=PROPERTY_DEFINITION('material property','density of part',#25674);
#14445=PROPERTY_DEFINITION('material property','material name',#25675);
#14446=PROPERTY_DEFINITION('material property','density of part',#25675);
#14447=PROPERTY_DEFINITION('material property','material name',#25676);
#14448=PROPERTY_DEFINITION('material property','density of part',#25676);
#14449=PROPERTY_DEFINITION('material property','material name',#25678);
#14450=PROPERTY_DEFINITION('material property','density of part',#25678);
#14451=PROPERTY_DEFINITION('material property','material name',#25679);
#14452=PROPERTY_DEFINITION('material property','density of part',#25679);
#14453=PROPERTY_DEFINITION('material property','material name',#25680);
#14454=PROPERTY_DEFINITION('material property','density of part',#25680);
#14455=PROPERTY_DEFINITION('material property','material name',#25681);
#14456=PROPERTY_DEFINITION('material property','density of part',#25681);
#14457=PROPERTY_DEFINITION('material property','material name',#25682);
#14458=PROPERTY_DEFINITION('material property','density of part',#25682);
#14459=PROPERTY_DEFINITION('material property','material name',#25683);
#14460=PROPERTY_DEFINITION('material property','density of part',#25683);
#14461=PROPERTY_DEFINITION('material property','material name',#25684);
#14462=PROPERTY_DEFINITION('material property','density of part',#25684);
#14463=PROPERTY_DEFINITION('material property','material name',#25685);
#14464=PROPERTY_DEFINITION('material property','density of part',#25685);
#14465=PROPERTY_DEFINITION('material property','material name',#25686);
#14466=PROPERTY_DEFINITION('material property','density of part',#25686);
#14467=PROPERTY_DEFINITION('material property','material name',#25687);
#14468=PROPERTY_DEFINITION('material property','density of part',#25687);
#14469=PROPERTY_DEFINITION('material property','material name',#25688);
#14470=PROPERTY_DEFINITION('material property','density of part',#25688);
#14471=PROPERTY_DEFINITION('material property','material name',#25690);
#14472=PROPERTY_DEFINITION('material property','density of part',#25690);
#14473=PROPERTY_DEFINITION('material property','material name',#25691);
#14474=PROPERTY_DEFINITION('material property','density of part',#25691);
#14475=PROPERTY_DEFINITION('material property','material name',#25692);
#14476=PROPERTY_DEFINITION('material property','density of part',#25692);
#14477=PROPERTY_DEFINITION('material property','material name',#25694);
#14478=PROPERTY_DEFINITION('material property','density of part',#25694);
#14479=PROPERTY_DEFINITION('material property','material name',#25695);
#14480=PROPERTY_DEFINITION('material property','density of part',#25695);
#14481=PROPERTY_DEFINITION('material property','material name',#25696);
#14482=PROPERTY_DEFINITION('material property','density of part',#25696);
#14483=PROPERTY_DEFINITION('material property','material name',#25697);
#14484=PROPERTY_DEFINITION('material property','density of part',#25697);
#14485=PROPERTY_DEFINITION('material property','material name',#25698);
#14486=PROPERTY_DEFINITION('material property','density of part',#25698);
#14487=PROPERTY_DEFINITION('material property','material name',#25699);
#14488=PROPERTY_DEFINITION('material property','density of part',#25699);
#14489=PROPERTY_DEFINITION('material property','material name',#25700);
#14490=PROPERTY_DEFINITION('material property','density of part',#25700);
#14491=PROPERTY_DEFINITION('material property','material name',#25701);
#14492=PROPERTY_DEFINITION('material property','density of part',#25701);
#14493=PROPERTY_DEFINITION('material property','material name',#25702);
#14494=PROPERTY_DEFINITION('material property','density of part',#25702);
#14495=PROPERTY_DEFINITION('material property','material name',#25703);
#14496=PROPERTY_DEFINITION('material property','density of part',#25703);
#14497=PROPERTY_DEFINITION('material property','material name',#25704);
#14498=PROPERTY_DEFINITION('material property','density of part',#25704);
#14499=PROPERTY_DEFINITION('material property','material name',#25705);
#14500=PROPERTY_DEFINITION('material property','density of part',#25705);
#14501=PROPERTY_DEFINITION('material property','material name',#25706);
#14502=PROPERTY_DEFINITION('material property','density of part',#25706);
#14503=PROPERTY_DEFINITION('material property','material name',#25707);
#14504=PROPERTY_DEFINITION('material property','density of part',#25707);
#14505=PROPERTY_DEFINITION('material property','material name',#25708);
#14506=PROPERTY_DEFINITION('material property','density of part',#25708);
#14507=PROPERTY_DEFINITION('material property','material name',#25709);
#14508=PROPERTY_DEFINITION('material property','density of part',#25709);
#14509=PROPERTY_DEFINITION('material property','material name',#25710);
#14510=PROPERTY_DEFINITION('material property','density of part',#25710);
#14511=PROPERTY_DEFINITION('material property','material name',#25712);
#14512=PROPERTY_DEFINITION('material property','density of part',#25712);
#14513=PROPERTY_DEFINITION('material property','material name',#25713);
#14514=PROPERTY_DEFINITION('material property','density of part',#25713);
#14515=PROPERTY_DEFINITION('material property','material name',#25714);
#14516=PROPERTY_DEFINITION('material property','density of part',#25714);
#14517=PROPERTY_DEFINITION('material property','material name',#25715);
#14518=PROPERTY_DEFINITION('material property','density of part',#25715);
#14519=PROPERTY_DEFINITION('material property','material name',#25716);
#14520=PROPERTY_DEFINITION('material property','density of part',#25716);
#14521=PROPERTY_DEFINITION('material property','material name',#25717);
#14522=PROPERTY_DEFINITION('material property','density of part',#25717);
#14523=PROPERTY_DEFINITION('material property','material name',#25718);
#14524=PROPERTY_DEFINITION('material property','density of part',#25718);
#14525=PROPERTY_DEFINITION('material property','material name',#25719);
#14526=PROPERTY_DEFINITION('material property','density of part',#25719);
#14527=PROPERTY_DEFINITION('material property','material name',#25720);
#14528=PROPERTY_DEFINITION('material property','density of part',#25720);
#14529=PROPERTY_DEFINITION('material property','material name',#25721);
#14530=PROPERTY_DEFINITION('material property','density of part',#25721);
#14531=PROPERTY_DEFINITION('material property','material name',#25722);
#14532=PROPERTY_DEFINITION('material property','density of part',#25722);
#14533=PROPERTY_DEFINITION('material property','material name',#25723);
#14534=PROPERTY_DEFINITION('material property','density of part',#25723);
#14535=PROPERTY_DEFINITION('material property','material name',#25724);
#14536=PROPERTY_DEFINITION('material property','density of part',#25724);
#14537=PROPERTY_DEFINITION('material property','material name',#25725);
#14538=PROPERTY_DEFINITION('material property','density of part',#25725);
#14539=PROPERTY_DEFINITION('material property','material name',#25726);
#14540=PROPERTY_DEFINITION('material property','density of part',#25726);
#14541=PROPERTY_DEFINITION('material property','material name',#25727);
#14542=PROPERTY_DEFINITION('material property','density of part',#25727);
#14543=PROPERTY_DEFINITION('material property','material name',#25728);
#14544=PROPERTY_DEFINITION('material property','density of part',#25728);
#14545=PROPERTY_DEFINITION('material property','material name',#25729);
#14546=PROPERTY_DEFINITION('material property','density of part',#25729);
#14547=PROPERTY_DEFINITION('material property','material name',#25730);
#14548=PROPERTY_DEFINITION('material property','density of part',#25730);
#14549=PROPERTY_DEFINITION('material property','material name',#25731);
#14550=PROPERTY_DEFINITION('material property','density of part',#25731);
#14551=PROPERTY_DEFINITION('material property','material name',#25732);
#14552=PROPERTY_DEFINITION('material property','density of part',#25732);
#14553=PROPERTY_DEFINITION('material property','material name',#25733);
#14554=PROPERTY_DEFINITION('material property','density of part',#25733);
#14555=PROPERTY_DEFINITION('material property','material name',#25734);
#14556=PROPERTY_DEFINITION('material property','density of part',#25734);
#14557=PROPERTY_DEFINITION('material property','material name',#25735);
#14558=PROPERTY_DEFINITION('material property','density of part',#25735);
#14559=PROPERTY_DEFINITION('material property','material name',#25736);
#14560=PROPERTY_DEFINITION('material property','density of part',#25736);
#14561=PROPERTY_DEFINITION('material property','material name',#25737);
#14562=PROPERTY_DEFINITION('material property','density of part',#25737);
#14563=PROPERTY_DEFINITION('material property','material name',#25739);
#14564=PROPERTY_DEFINITION('material property','density of part',#25739);
#14565=PROPERTY_DEFINITION('material property','material name',#25740);
#14566=PROPERTY_DEFINITION('material property','density of part',#25740);
#14567=PROPERTY_DEFINITION('material property','material name',#25741);
#14568=PROPERTY_DEFINITION('material property','density of part',#25741);
#14569=PROPERTY_DEFINITION('material property','material name',#25742);
#14570=PROPERTY_DEFINITION('material property','density of part',#25742);
#14571=PROPERTY_DEFINITION('material property','material name',#25743);
#14572=PROPERTY_DEFINITION('material property','density of part',#25743);
#14573=PROPERTY_DEFINITION('material property','material name',#25745);
#14574=PROPERTY_DEFINITION('material property','density of part',#25745);
#14575=PROPERTY_DEFINITION('material property','material name',#25746);
#14576=PROPERTY_DEFINITION('material property','density of part',#25746);
#14577=PROPERTY_DEFINITION('material property','material name',#25747);
#14578=PROPERTY_DEFINITION('material property','density of part',#25747);
#14579=PROPERTY_DEFINITION('material property','material name',#25748);
#14580=PROPERTY_DEFINITION('material property','density of part',#25748);
#14581=PROPERTY_DEFINITION('material property','material name',#25749);
#14582=PROPERTY_DEFINITION('material property','density of part',#25749);
#14583=PROPERTY_DEFINITION('material property','material name',#25750);
#14584=PROPERTY_DEFINITION('material property','density of part',#25750);
#14585=AXIS2_PLACEMENT_3D('',#20974,#16468,#16469);
#14586=AXIS2_PLACEMENT_3D('',#20975,#16470,#16471);
#14587=AXIS2_PLACEMENT_3D('',#20976,#16472,#16473);
#14588=AXIS2_PLACEMENT_3D('',#20977,#16474,#16475);
#14589=AXIS2_PLACEMENT_3D('',#20979,#16476,#16477);
#14590=AXIS2_PLACEMENT_3D('',#20982,#16479,#16480);
#14591=AXIS2_PLACEMENT_3D('',#20983,#16481,#16482);
#14592=AXIS2_PLACEMENT_3D('',#20985,#16483,#16484);
#14593=AXIS2_PLACEMENT_3D('',#20988,#16486,#16487);
#14594=AXIS2_PLACEMENT_3D('',#20989,#16488,#16489);
#14595=AXIS2_PLACEMENT_3D('',#20991,#16490,#16491);
#14596=AXIS2_PLACEMENT_3D('',#20994,#16493,#16494);
#14597=AXIS2_PLACEMENT_3D('',#20995,#16495,#16496);
#14598=AXIS2_PLACEMENT_3D('',#20997,#16497,#16498);
#14599=AXIS2_PLACEMENT_3D('',#21000,#16500,#16501);
#14600=AXIS2_PLACEMENT_3D('',#21001,#16502,#16503);
#14601=AXIS2_PLACEMENT_3D('',#21003,#16504,#16505);
#14602=AXIS2_PLACEMENT_3D('',#21006,#16507,#16508);
#14603=AXIS2_PLACEMENT_3D('',#21007,#16509,#16510);
#14604=AXIS2_PLACEMENT_3D('',#21009,#16511,#16512);
#14605=AXIS2_PLACEMENT_3D('',#21012,#16514,#16515);
#14606=AXIS2_PLACEMENT_3D('',#21013,#16516,#16517);
#14607=AXIS2_PLACEMENT_3D('',#21015,#16518,#16519);
#14608=AXIS2_PLACEMENT_3D('',#21018,#16521,#16522);
#14609=AXIS2_PLACEMENT_3D('',#21019,#16523,#16524);
#14610=AXIS2_PLACEMENT_3D('',#21021,#16525,#16526);
#14611=AXIS2_PLACEMENT_3D('',#21024,#16528,#16529);
#14612=AXIS2_PLACEMENT_3D('',#21025,#16530,#16531);
#14613=AXIS2_PLACEMENT_3D('',#21034,#16536,#16537);
#14614=AXIS2_PLACEMENT_3D('',#21040,#16541,#16542);
#14615=AXIS2_PLACEMENT_3D('',#21046,#16546,#16547);
#14616=AXIS2_PLACEMENT_3D('',#21049,#16550,#16551);
#14617=AXIS2_PLACEMENT_3D('',#21050,#16552,#16553);
#14618=AXIS2_PLACEMENT_3D('',#21051,#16554,#16555);
#14619=AXIS2_PLACEMENT_3D('',#21052,#16556,#16557);
#14620=AXIS2_PLACEMENT_3D('',#21061,#16562,#16563);
#14621=AXIS2_PLACEMENT_3D('',#21067,#16567,#16568);
#14622=AXIS2_PLACEMENT_3D('',#21073,#16572,#16573);
#14623=AXIS2_PLACEMENT_3D('',#21076,#16576,#16577);
#14624=AXIS2_PLACEMENT_3D('',#21077,#16578,#16579);
#14625=AXIS2_PLACEMENT_3D('',#21078,#16580,#16581);
#14626=AXIS2_PLACEMENT_3D('',#21079,#16582,#16583);
#14627=AXIS2_PLACEMENT_3D('',#21088,#16588,#16589);
#14628=AXIS2_PLACEMENT_3D('',#21094,#16593,#16594);
#14629=AXIS2_PLACEMENT_3D('',#21100,#16598,#16599);
#14630=AXIS2_PLACEMENT_3D('',#21103,#16602,#16603);
#14631=AXIS2_PLACEMENT_3D('',#21104,#16604,#16605);
#14632=AXIS2_PLACEMENT_3D('',#21105,#16606,#16607);
#14633=AXIS2_PLACEMENT_3D('',#21106,#16608,#16609);
#14634=AXIS2_PLACEMENT_3D('',#21108,#16610,#16611);
#14635=AXIS2_PLACEMENT_3D('',#21111,#16613,#16614);
#14636=AXIS2_PLACEMENT_3D('',#21112,#16615,#16616);
#14637=AXIS2_PLACEMENT_3D('',#21114,#16617,#16618);
#14638=AXIS2_PLACEMENT_3D('',#21117,#16620,#16621);
#14639=AXIS2_PLACEMENT_3D('',#21118,#16622,#16623);
#14640=AXIS2_PLACEMENT_3D('',#21120,#16624,#16625);
#14641=AXIS2_PLACEMENT_3D('',#21123,#16627,#16628);
#14642=AXIS2_PLACEMENT_3D('',#21124,#16629,#16630);
#14643=AXIS2_PLACEMENT_3D('',#21126,#16631,#16632);
#14644=AXIS2_PLACEMENT_3D('',#21129,#16634,#16635);
#14645=AXIS2_PLACEMENT_3D('',#21130,#16636,#16637);
#14646=AXIS2_PLACEMENT_3D('',#21132,#16638,#16639);
#14647=AXIS2_PLACEMENT_3D('',#21135,#16641,#16642);
#14648=AXIS2_PLACEMENT_3D('',#21136,#16643,#16644);
#14649=AXIS2_PLACEMENT_3D('',#21138,#16645,#16646);
#14650=AXIS2_PLACEMENT_3D('',#21141,#16648,#16649);
#14651=AXIS2_PLACEMENT_3D('',#21142,#16650,#16651);
#14652=AXIS2_PLACEMENT_3D('',#21144,#16652,#16653);
#14653=AXIS2_PLACEMENT_3D('',#21147,#16655,#16656);
#14654=AXIS2_PLACEMENT_3D('',#21148,#16657,#16658);
#14655=AXIS2_PLACEMENT_3D('',#21150,#16659,#16660);
#14656=AXIS2_PLACEMENT_3D('',#21153,#16662,#16663);
#14657=AXIS2_PLACEMENT_3D('',#21154,#16664,#16665);
#14658=AXIS2_PLACEMENT_3D('',#21156,#16666,#16667);
#14659=AXIS2_PLACEMENT_3D('',#21159,#16669,#16670);
#14660=AXIS2_PLACEMENT_3D('',#21160,#16671,#16672);
#14661=AXIS2_PLACEMENT_3D('',#21169,#16677,#16678);
#14662=AXIS2_PLACEMENT_3D('',#21178,#16683,#16684);
#14663=AXIS2_PLACEMENT_3D('',#21184,#16688,#16689);
#14664=AXIS2_PLACEMENT_3D('',#21190,#16693,#16694);
#14665=AXIS2_PLACEMENT_3D('',#21198,#16699,#16700);
#14666=AXIS2_PLACEMENT_3D('',#21199,#16701,#16702);
#14667=AXIS2_PLACEMENT_3D('',#21204,#16705,#16706);
#14668=AXIS2_PLACEMENT_3D('',#21206,#16707,#16708);
#14669=AXIS2_PLACEMENT_3D('',#21207,#16709,#16710);
#14670=AXIS2_PLACEMENT_3D('',#21209,#16711,#16712);
#14671=AXIS2_PLACEMENT_3D('',#21211,#16714,#16715);
#14672=AXIS2_PLACEMENT_3D('',#21214,#16717,#16718);
#14673=AXIS2_PLACEMENT_3D('',#21215,#16719,#16720);
#14674=AXIS2_PLACEMENT_3D('',#21218,#16722,#16723);
#14675=AXIS2_PLACEMENT_3D('',#21219,#16724,#16725);
#14676=AXIS2_PLACEMENT_3D('',#21223,#16728,#16729);
#14677=AXIS2_PLACEMENT_3D('',#21226,#16732,#16733);
#14678=AXIS2_PLACEMENT_3D('',#21227,#16734,#16735);
#14679=AXIS2_PLACEMENT_3D('',#21228,#16736,#16737);
#14680=AXIS2_PLACEMENT_3D('',#21229,#16738,#16739);
#14681=AXIS2_PLACEMENT_3D('',#21231,#16740,#16741);
#14682=AXIS2_PLACEMENT_3D('',#21234,#16743,#16744);
#14683=AXIS2_PLACEMENT_3D('',#21235,#16745,#16746);
#14684=AXIS2_PLACEMENT_3D('',#21237,#16747,#16748);
#14685=AXIS2_PLACEMENT_3D('',#21240,#16750,#16751);
#14686=AXIS2_PLACEMENT_3D('',#21241,#16752,#16753);
#14687=AXIS2_PLACEMENT_3D('',#21243,#16754,#16755);
#14688=AXIS2_PLACEMENT_3D('',#21246,#16757,#16758);
#14689=AXIS2_PLACEMENT_3D('',#21247,#16759,#16760);
#14690=AXIS2_PLACEMENT_3D('',#21249,#16761,#16762);
#14691=AXIS2_PLACEMENT_3D('',#21252,#16764,#16765);
#14692=AXIS2_PLACEMENT_3D('',#21253,#16766,#16767);
#14693=AXIS2_PLACEMENT_3D('',#21255,#16768,#16769);
#14694=AXIS2_PLACEMENT_3D('',#21258,#16771,#16772);
#14695=AXIS2_PLACEMENT_3D('',#21259,#16773,#16774);
#14696=AXIS2_PLACEMENT_3D('',#21261,#16775,#16776);
#14697=AXIS2_PLACEMENT_3D('',#21262,#16777,#16778);
#14698=AXIS2_PLACEMENT_3D('',#21265,#16780,#16781);
#14699=AXIS2_PLACEMENT_3D('',#21266,#16782,#16783);
#14700=AXIS2_PLACEMENT_3D('',#21268,#16784,#16785);
#14701=AXIS2_PLACEMENT_3D('',#21271,#16787,#16788);
#14702=AXIS2_PLACEMENT_3D('',#21272,#16789,#16790);
#14703=AXIS2_PLACEMENT_3D('',#21273,#16791,#16792);
#14704=AXIS2_PLACEMENT_3D('',#21274,#16793,#16794);
#14705=AXIS2_PLACEMENT_3D('',#21275,#16795,#16796);
#14706=AXIS2_PLACEMENT_3D('',#21277,#16797,#16798);
#14707=AXIS2_PLACEMENT_3D('',#21280,#16800,#16801);
#14708=AXIS2_PLACEMENT_3D('',#21281,#16802,#16803);
#14709=AXIS2_PLACEMENT_3D('',#21283,#16804,#16805);
#14710=AXIS2_PLACEMENT_3D('',#21286,#16807,#16808);
#14711=AXIS2_PLACEMENT_3D('',#21287,#16809,#16810);
#14712=AXIS2_PLACEMENT_3D('',#21289,#16811,#16812);
#14713=AXIS2_PLACEMENT_3D('',#21292,#16814,#16815);
#14714=AXIS2_PLACEMENT_3D('',#21293,#16816,#16817);
#14715=AXIS2_PLACEMENT_3D('',#21295,#16818,#16819);
#14716=AXIS2_PLACEMENT_3D('',#21298,#16821,#16822);
#14717=AXIS2_PLACEMENT_3D('',#21299,#16823,#16824);
#14718=AXIS2_PLACEMENT_3D('',#21301,#16825,#16826);
#14719=AXIS2_PLACEMENT_3D('',#21304,#16828,#16829);
#14720=AXIS2_PLACEMENT_3D('',#21305,#16830,#16831);
#14721=AXIS2_PLACEMENT_3D('',#21307,#16832,#16833);
#14722=AXIS2_PLACEMENT_3D('',#21308,#16834,#16835);
#14723=AXIS2_PLACEMENT_3D('',#21310,#16836,#16837);
#14724=AXIS2_PLACEMENT_3D('',#21312,#16839,#16840);
#14725=AXIS2_PLACEMENT_3D('',#21314,#16841,#16842);
#14726=AXIS2_PLACEMENT_3D('',#21317,#16844,#16845);
#14727=AXIS2_PLACEMENT_3D('',#21318,#16846,#16847);
#14728=AXIS2_PLACEMENT_3D('',#21319,#16848,#16849);
#14729=AXIS2_PLACEMENT_3D('',#21320,#16850,#16851);
#14730=AXIS2_PLACEMENT_3D('',#21321,#16852,#16853);
#14731=AXIS2_PLACEMENT_3D('',#21323,#16854,#16855);
#14732=AXIS2_PLACEMENT_3D('',#21326,#16857,#16858);
#14733=AXIS2_PLACEMENT_3D('',#21327,#16859,#16860);
#14734=AXIS2_PLACEMENT_3D('',#21329,#16861,#16862);
#14735=AXIS2_PLACEMENT_3D('',#21332,#16864,#16865);
#14736=AXIS2_PLACEMENT_3D('',#21333,#16866,#16867);
#14737=AXIS2_PLACEMENT_3D('',#21335,#16868,#16869);
#14738=AXIS2_PLACEMENT_3D('',#21338,#16871,#16872);
#14739=AXIS2_PLACEMENT_3D('',#21339,#16873,#16874);
#14740=AXIS2_PLACEMENT_3D('',#21341,#16875,#16876);
#14741=AXIS2_PLACEMENT_3D('',#21344,#16878,#16879);
#14742=AXIS2_PLACEMENT_3D('',#21345,#16880,#16881);
#14743=AXIS2_PLACEMENT_3D('',#21347,#16882,#16883);
#14744=AXIS2_PLACEMENT_3D('',#21350,#16885,#16886);
#14745=AXIS2_PLACEMENT_3D('',#21351,#16887,#16888);
#14746=AXIS2_PLACEMENT_3D('',#21353,#16889,#16890);
#14747=AXIS2_PLACEMENT_3D('',#21356,#16892,#16893);
#14748=AXIS2_PLACEMENT_3D('',#21357,#16894,#16895);
#14749=AXIS2_PLACEMENT_3D('',#21359,#16896,#16897);
#14750=AXIS2_PLACEMENT_3D('',#21362,#16899,#16900);
#14751=AXIS2_PLACEMENT_3D('',#21363,#16901,#16902);
#14752=AXIS2_PLACEMENT_3D('',#21365,#16903,#16904);
#14753=AXIS2_PLACEMENT_3D('',#21368,#16906,#16907);
#14754=AXIS2_PLACEMENT_3D('',#21369,#16908,#16909);
#14755=AXIS2_PLACEMENT_3D('',#21371,#16910,#16911);
#14756=AXIS2_PLACEMENT_3D('',#21374,#16913,#16914);
#14757=AXIS2_PLACEMENT_3D('',#21375,#16915,#16916);
#14758=AXIS2_PLACEMENT_3D('',#21384,#16921,#16922);
#14759=AXIS2_PLACEMENT_3D('',#21393,#16927,#16928);
#14760=AXIS2_PLACEMENT_3D('',#21399,#16932,#16933);
#14761=AXIS2_PLACEMENT_3D('',#21405,#16937,#16938);
#14762=AXIS2_PLACEMENT_3D('',#21412,#16943,#16944);
#14763=AXIS2_PLACEMENT_3D('',#21417,#16947,#16948);
#14764=AXIS2_PLACEMENT_3D('',#21419,#16949,#16950);
#14765=AXIS2_PLACEMENT_3D('',#21420,#16951,#16952);
#14766=AXIS2_PLACEMENT_3D('',#21423,#16954,#16955);
#14767=AXIS2_PLACEMENT_3D('',#21424,#16956,#16957);
#14768=AXIS2_PLACEMENT_3D('',#21427,#16959,#16960);
#14769=AXIS2_PLACEMENT_3D('',#21428,#16961,#16962);
#14770=AXIS2_PLACEMENT_3D('',#21432,#16965,#16966);
#14771=AXIS2_PLACEMENT_3D('',#21435,#16969,#16970);
#14772=AXIS2_PLACEMENT_3D('',#21436,#16971,#16972);
#14773=AXIS2_PLACEMENT_3D('',#21437,#16973,#16974);
#14774=AXIS2_PLACEMENT_3D('',#21438,#16975,#16976);
#14775=AXIS2_PLACEMENT_3D('',#21440,#16977,#16978);
#14776=AXIS2_PLACEMENT_3D('',#21443,#16980,#16981);
#14777=AXIS2_PLACEMENT_3D('',#21444,#16982,#16983);
#14778=AXIS2_PLACEMENT_3D('',#21446,#16984,#16985);
#14779=AXIS2_PLACEMENT_3D('',#21449,#16987,#16988);
#14780=AXIS2_PLACEMENT_3D('',#21450,#16989,#16990);
#14781=AXIS2_PLACEMENT_3D('',#21452,#16991,#16992);
#14782=AXIS2_PLACEMENT_3D('',#21455,#16994,#16995);
#14783=AXIS2_PLACEMENT_3D('',#21456,#16996,#16997);
#14784=AXIS2_PLACEMENT_3D('',#21458,#16998,#16999);
#14785=AXIS2_PLACEMENT_3D('',#21461,#17001,#17002);
#14786=AXIS2_PLACEMENT_3D('',#21462,#17003,#17004);
#14787=AXIS2_PLACEMENT_3D('',#21464,#17005,#17006);
#14788=AXIS2_PLACEMENT_3D('',#21467,#17008,#17009);
#14789=AXIS2_PLACEMENT_3D('',#21468,#17010,#17011);
#14790=AXIS2_PLACEMENT_3D('',#21470,#17012,#17013);
#14791=AXIS2_PLACEMENT_3D('',#21471,#17014,#17015);
#14792=AXIS2_PLACEMENT_3D('',#21474,#17017,#17018);
#14793=AXIS2_PLACEMENT_3D('',#21475,#17019,#17020);
#14794=AXIS2_PLACEMENT_3D('',#21477,#17021,#17022);
#14795=AXIS2_PLACEMENT_3D('',#21480,#17024,#17025);
#14796=AXIS2_PLACEMENT_3D('',#21481,#17026,#17027);
#14797=AXIS2_PLACEMENT_3D('',#21482,#17028,#17029);
#14798=AXIS2_PLACEMENT_3D('',#21483,#17030,#17031);
#14799=AXIS2_PLACEMENT_3D('',#21484,#17032,#17033);
#14800=AXIS2_PLACEMENT_3D('',#21486,#17034,#17035);
#14801=AXIS2_PLACEMENT_3D('',#21489,#17037,#17038);
#14802=AXIS2_PLACEMENT_3D('',#21490,#17039,#17040);
#14803=AXIS2_PLACEMENT_3D('',#21492,#17041,#17042);
#14804=AXIS2_PLACEMENT_3D('',#21495,#17044,#17045);
#14805=AXIS2_PLACEMENT_3D('',#21496,#17046,#17047);
#14806=AXIS2_PLACEMENT_3D('',#21498,#17048,#17049);
#14807=AXIS2_PLACEMENT_3D('',#21501,#17051,#17052);
#14808=AXIS2_PLACEMENT_3D('',#21502,#17053,#17054);
#14809=AXIS2_PLACEMENT_3D('',#21504,#17055,#17056);
#14810=AXIS2_PLACEMENT_3D('',#21507,#17058,#17059);
#14811=AXIS2_PLACEMENT_3D('',#21508,#17060,#17061);
#14812=AXIS2_PLACEMENT_3D('',#21510,#17062,#17063);
#14813=AXIS2_PLACEMENT_3D('',#21513,#17065,#17066);
#14814=AXIS2_PLACEMENT_3D('',#21514,#17067,#17068);
#14815=AXIS2_PLACEMENT_3D('',#21516,#17069,#17070);
#14816=AXIS2_PLACEMENT_3D('',#21517,#17071,#17072);
#14817=AXIS2_PLACEMENT_3D('',#21519,#17073,#17074);
#14818=AXIS2_PLACEMENT_3D('',#21521,#17076,#17077);
#14819=AXIS2_PLACEMENT_3D('',#21523,#17078,#17079);
#14820=AXIS2_PLACEMENT_3D('',#21526,#17081,#17082);
#14821=AXIS2_PLACEMENT_3D('',#21527,#17083,#17084);
#14822=AXIS2_PLACEMENT_3D('',#21528,#17085,#17086);
#14823=AXIS2_PLACEMENT_3D('',#21529,#17087,#17088);
#14824=AXIS2_PLACEMENT_3D('',#21530,#17089,#17090);
#14825=AXIS2_PLACEMENT_3D('',#21532,#17091,#17092);
#14826=AXIS2_PLACEMENT_3D('',#21535,#17094,#17095);
#14827=AXIS2_PLACEMENT_3D('',#21536,#17096,#17097);
#14828=AXIS2_PLACEMENT_3D('',#21537,#17098,#17099);
#14829=AXIS2_PLACEMENT_3D('',#21538,#17100,#17101);
#14830=AXIS2_PLACEMENT_3D('',#21539,#17102,#17103);
#14831=AXIS2_PLACEMENT_3D('',#21541,#17104,#17105);
#14832=AXIS2_PLACEMENT_3D('',#21544,#17107,#17108);
#14833=AXIS2_PLACEMENT_3D('',#21545,#17109,#17110);
#14834=AXIS2_PLACEMENT_3D('',#21546,#17111,#17112);
#14835=AXIS2_PLACEMENT_3D('',#21547,#17113,#17114);
#14836=AXIS2_PLACEMENT_3D('',#21548,#17115,#17116);
#14837=AXIS2_PLACEMENT_3D('',#21550,#17117,#17118);
#14838=AXIS2_PLACEMENT_3D('',#21553,#17120,#17121);
#14839=AXIS2_PLACEMENT_3D('',#21554,#17122,#17123);
#14840=AXIS2_PLACEMENT_3D('',#21555,#17124,#17125);
#14841=AXIS2_PLACEMENT_3D('',#21557,#17126,#17127);
#14842=AXIS2_PLACEMENT_3D('',#21560,#17129,#17130);
#14843=AXIS2_PLACEMENT_3D('',#21561,#17131,#17132);
#14844=AXIS2_PLACEMENT_3D('',#21562,#17133,#17134);
#14845=AXIS2_PLACEMENT_3D('',#21564,#17135,#17136);
#14846=AXIS2_PLACEMENT_3D('',#21567,#17138,#17139);
#14847=AXIS2_PLACEMENT_3D('',#21568,#17140,#17141);
#14848=AXIS2_PLACEMENT_3D('',#21569,#17142,#17143);
#14849=AXIS2_PLACEMENT_3D('',#21570,#17144,#17145);
#14850=AXIS2_PLACEMENT_3D('',#21571,#17146,#17147);
#14851=AXIS2_PLACEMENT_3D('',#21573,#17148,#17149);
#14852=AXIS2_PLACEMENT_3D('',#21576,#17151,#17152);
#14853=AXIS2_PLACEMENT_3D('',#21577,#17153,#17154);
#14854=AXIS2_PLACEMENT_3D('',#21579,#17155,#17156);
#14855=AXIS2_PLACEMENT_3D('',#21582,#17158,#17159);
#14856=AXIS2_PLACEMENT_3D('',#21583,#17160,#17161);
#14857=AXIS2_PLACEMENT_3D('',#21584,#17162,#17163);
#14858=AXIS2_PLACEMENT_3D('',#21585,#17164,#17165);
#14859=AXIS2_PLACEMENT_3D('',#21586,#17166,#17167);
#14860=AXIS2_PLACEMENT_3D('',#21588,#17168,#17169);
#14861=AXIS2_PLACEMENT_3D('',#21591,#17171,#17172);
#14862=AXIS2_PLACEMENT_3D('',#21592,#17173,#17174);
#14863=AXIS2_PLACEMENT_3D('',#21594,#17175,#17176);
#14864=AXIS2_PLACEMENT_3D('',#21597,#17178,#17179);
#14865=AXIS2_PLACEMENT_3D('',#21598,#17180,#17181);
#14866=AXIS2_PLACEMENT_3D('',#21599,#17182,#17183);
#14867=AXIS2_PLACEMENT_3D('',#21600,#17184,#17185);
#14868=AXIS2_PLACEMENT_3D('',#21601,#17186,#17187);
#14869=AXIS2_PLACEMENT_3D('',#21603,#17188,#17189);
#14870=AXIS2_PLACEMENT_3D('',#21606,#17191,#17192);
#14871=AXIS2_PLACEMENT_3D('',#21607,#17193,#17194);
#14872=AXIS2_PLACEMENT_3D('',#21609,#17195,#17196);
#14873=AXIS2_PLACEMENT_3D('',#21612,#17198,#17199);
#14874=AXIS2_PLACEMENT_3D('',#21613,#17200,#17201);
#14875=AXIS2_PLACEMENT_3D('',#21614,#17202,#17203);
#14876=AXIS2_PLACEMENT_3D('',#21615,#17204,#17205);
#14877=AXIS2_PLACEMENT_3D('',#21616,#17206,#17207);
#14878=AXIS2_PLACEMENT_3D('',#21618,#17208,#17209);
#14879=AXIS2_PLACEMENT_3D('',#21621,#17211,#17212);
#14880=AXIS2_PLACEMENT_3D('',#21622,#17213,#17214);
#14881=AXIS2_PLACEMENT_3D('',#21624,#17215,#17216);
#14882=AXIS2_PLACEMENT_3D('',#21627,#17218,#17219);
#14883=AXIS2_PLACEMENT_3D('',#21628,#17220,#17221);
#14884=AXIS2_PLACEMENT_3D('',#21629,#17222,#17223);
#14885=AXIS2_PLACEMENT_3D('',#21630,#17224,#17225);
#14886=AXIS2_PLACEMENT_3D('',#21631,#17226,#17227);
#14887=AXIS2_PLACEMENT_3D('',#21633,#17228,#17229);
#14888=AXIS2_PLACEMENT_3D('',#21636,#17231,#17232);
#14889=AXIS2_PLACEMENT_3D('',#21637,#17233,#17234);
#14890=AXIS2_PLACEMENT_3D('',#21639,#17235,#17236);
#14891=AXIS2_PLACEMENT_3D('',#21642,#17238,#17239);
#14892=AXIS2_PLACEMENT_3D('',#21643,#17240,#17241);
#14893=AXIS2_PLACEMENT_3D('',#21644,#17242,#17243);
#14894=AXIS2_PLACEMENT_3D('',#21645,#17244,#17245);
#14895=AXIS2_PLACEMENT_3D('',#21646,#17246,#17247);
#14896=AXIS2_PLACEMENT_3D('',#21655,#17252,#17253);
#14897=AXIS2_PLACEMENT_3D('',#21661,#17257,#17258);
#14898=AXIS2_PLACEMENT_3D('',#21667,#17262,#17263);
#14899=AXIS2_PLACEMENT_3D('',#21673,#17267,#17268);
#14900=AXIS2_PLACEMENT_3D('',#21679,#17272,#17273);
#14901=AXIS2_PLACEMENT_3D('',#21682,#17276,#17277);
#14902=AXIS2_PLACEMENT_3D('',#21683,#17278,#17279);
#14903=AXIS2_PLACEMENT_3D('',#21684,#17280,#17281);
#14904=AXIS2_PLACEMENT_3D('',#21686,#17282,#17283);
#14905=AXIS2_PLACEMENT_3D('',#21687,#17284,#17285);
#14906=AXIS2_PLACEMENT_3D('',#21689,#17286,#17287);
#14907=AXIS2_PLACEMENT_3D('',#21690,#17288,#17289);
#14908=AXIS2_PLACEMENT_3D('',#21692,#17290,#17291);
#14909=AXIS2_PLACEMENT_3D('',#21694,#17293,#17294);
#14910=AXIS2_PLACEMENT_3D('',#21696,#17295,#17296);
#14911=AXIS2_PLACEMENT_3D('',#21698,#17298,#17299);
#14912=AXIS2_PLACEMENT_3D('',#21700,#17300,#17301);
#14913=AXIS2_PLACEMENT_3D('',#21702,#17303,#17304);
#14914=AXIS2_PLACEMENT_3D('',#21704,#17305,#17306);
#14915=AXIS2_PLACEMENT_3D('',#21705,#17307,#17308);
#14916=AXIS2_PLACEMENT_3D('',#21707,#17309,#17310);
#14917=AXIS2_PLACEMENT_3D('',#21709,#17312,#17313);
#14918=AXIS2_PLACEMENT_3D('',#21711,#17315,#17316);
#14919=AXIS2_PLACEMENT_3D('',#21712,#17317,#17318);
#14920=AXIS2_PLACEMENT_3D('',#21713,#17319,#17320);
#14921=AXIS2_PLACEMENT_3D('',#21715,#17321,#17322);
#14922=AXIS2_PLACEMENT_3D('',#21718,#17324,#17325);
#14923=AXIS2_PLACEMENT_3D('',#21719,#17326,#17327);
#14924=AXIS2_PLACEMENT_3D('',#21721,#17328,#17329);
#14925=AXIS2_PLACEMENT_3D('',#21724,#17331,#17332);
#14926=AXIS2_PLACEMENT_3D('',#21725,#17333,#17334);
#14927=AXIS2_PLACEMENT_3D('',#21727,#17335,#17336);
#14928=AXIS2_PLACEMENT_3D('',#21730,#17338,#17339);
#14929=AXIS2_PLACEMENT_3D('',#21731,#17340,#17341);
#14930=AXIS2_PLACEMENT_3D('',#21733,#17342,#17343);
#14931=AXIS2_PLACEMENT_3D('',#21736,#17345,#17346);
#14932=AXIS2_PLACEMENT_3D('',#21737,#17347,#17348);
#14933=AXIS2_PLACEMENT_3D('',#21739,#17349,#17350);
#14934=AXIS2_PLACEMENT_3D('',#21742,#17352,#17353);
#14935=AXIS2_PLACEMENT_3D('',#21743,#17354,#17355);
#14936=AXIS2_PLACEMENT_3D('',#21745,#17356,#17357);
#14937=AXIS2_PLACEMENT_3D('',#21748,#17359,#17360);
#14938=AXIS2_PLACEMENT_3D('',#21749,#17361,#17362);
#14939=AXIS2_PLACEMENT_3D('',#21751,#17363,#17364);
#14940=AXIS2_PLACEMENT_3D('',#21754,#17366,#17367);
#14941=AXIS2_PLACEMENT_3D('',#21755,#17368,#17369);
#14942=AXIS2_PLACEMENT_3D('',#21757,#17370,#17371);
#14943=AXIS2_PLACEMENT_3D('',#21760,#17373,#17374);
#14944=AXIS2_PLACEMENT_3D('',#21761,#17375,#17376);
#14945=AXIS2_PLACEMENT_3D('',#21770,#17381,#17382);
#14946=AXIS2_PLACEMENT_3D('',#21776,#17386,#17387);
#14947=AXIS2_PLACEMENT_3D('',#21782,#17391,#17392);
#14948=AXIS2_PLACEMENT_3D('',#21785,#17395,#17396);
#14949=AXIS2_PLACEMENT_3D('',#21786,#17397,#17398);
#14950=AXIS2_PLACEMENT_3D('',#21787,#17399,#17400);
#14951=AXIS2_PLACEMENT_3D('',#21788,#17401,#17402);
#14952=AXIS2_PLACEMENT_3D('',#21790,#17403,#17404);
#14953=AXIS2_PLACEMENT_3D('',#21793,#17406,#17407);
#14954=AXIS2_PLACEMENT_3D('',#21794,#17408,#17409);
#14955=AXIS2_PLACEMENT_3D('',#21796,#17410,#17411);
#14956=AXIS2_PLACEMENT_3D('',#21799,#17413,#17414);
#14957=AXIS2_PLACEMENT_3D('',#21800,#17415,#17416);
#14958=AXIS2_PLACEMENT_3D('',#21802,#17417,#17418);
#14959=AXIS2_PLACEMENT_3D('',#21805,#17420,#17421);
#14960=AXIS2_PLACEMENT_3D('',#21806,#17422,#17423);
#14961=AXIS2_PLACEMENT_3D('',#21808,#17424,#17425);
#14962=AXIS2_PLACEMENT_3D('',#21811,#17427,#17428);
#14963=AXIS2_PLACEMENT_3D('',#21812,#17429,#17430);
#14964=AXIS2_PLACEMENT_3D('',#21829,#17439,#17440);
#14965=AXIS2_PLACEMENT_3D('',#21835,#17444,#17445);
#14966=AXIS2_PLACEMENT_3D('',#21839,#17448,#17449);
#14967=AXIS2_PLACEMENT_3D('',#21843,#17452,#17453);
#14968=AXIS2_PLACEMENT_3D('',#21845,#17455,#17456);
#14969=AXIS2_PLACEMENT_3D('',#21852,#17460,#17461);
#14970=AXIS2_PLACEMENT_3D('',#21853,#17462,#17463);
#14971=AXIS2_PLACEMENT_3D('',#21858,#17466,#17467);
#14972=AXIS2_PLACEMENT_3D('',#21860,#17468,#17469);
#14973=AXIS2_PLACEMENT_3D('',#21861,#17470,#17471);
#14974=AXIS2_PLACEMENT_3D('',#21864,#17473,#17474);
#14975=AXIS2_PLACEMENT_3D('',#21865,#17475,#17476);
#14976=AXIS2_PLACEMENT_3D('',#21868,#17478,#17479);
#14977=AXIS2_PLACEMENT_3D('',#21869,#17480,#17481);
#14978=AXIS2_PLACEMENT_3D('',#21872,#17483,#17484);
#14979=AXIS2_PLACEMENT_3D('',#21873,#17485,#17486);
#14980=AXIS2_PLACEMENT_3D('',#21877,#17489,#17490);
#14981=AXIS2_PLACEMENT_3D('',#21879,#17492,#17493);
#14982=AXIS2_PLACEMENT_3D('',#21880,#17494,#17495);
#14983=AXIS2_PLACEMENT_3D('',#21881,#17496,#17497);
#14984=AXIS2_PLACEMENT_3D('',#21882,#17498,#17499);
#14985=AXIS2_PLACEMENT_3D('',#21884,#17500,#17501);
#14986=AXIS2_PLACEMENT_3D('',#21887,#17503,#17504);
#14987=AXIS2_PLACEMENT_3D('',#21888,#17505,#17506);
#14988=AXIS2_PLACEMENT_3D('',#21890,#17507,#17508);
#14989=AXIS2_PLACEMENT_3D('',#21893,#17510,#17511);
#14990=AXIS2_PLACEMENT_3D('',#21894,#17512,#17513);
#14991=AXIS2_PLACEMENT_3D('',#21896,#17514,#17515);
#14992=AXIS2_PLACEMENT_3D('',#21899,#17517,#17518);
#14993=AXIS2_PLACEMENT_3D('',#21900,#17519,#17520);
#14994=AXIS2_PLACEMENT_3D('',#21902,#17521,#17522);
#14995=AXIS2_PLACEMENT_3D('',#21905,#17524,#17525);
#14996=AXIS2_PLACEMENT_3D('',#21906,#17526,#17527);
#14997=AXIS2_PLACEMENT_3D('',#21915,#17532,#17533);
#14998=AXIS2_PLACEMENT_3D('',#21924,#17538,#17539);
#14999=AXIS2_PLACEMENT_3D('',#21930,#17543,#17544);
#15000=AXIS2_PLACEMENT_3D('',#21936,#17548,#17549);
#15001=AXIS2_PLACEMENT_3D('',#21943,#17553,#17554);
#15002=AXIS2_PLACEMENT_3D('',#21945,#17555,#17556);
#15003=AXIS2_PLACEMENT_3D('',#21946,#17557,#17558);
#15004=AXIS2_PLACEMENT_3D('',#21951,#17562,#17563);
#15005=AXIS2_PLACEMENT_3D('',#21953,#17564,#17565);
#15006=AXIS2_PLACEMENT_3D('',#21955,#17567,#17568);
#15007=AXIS2_PLACEMENT_3D('',#21957,#17569,#17570);
#15008=AXIS2_PLACEMENT_3D('',#21959,#17572,#17573);
#15009=AXIS2_PLACEMENT_3D('',#21964,#17577,#17578);
#15010=AXIS2_PLACEMENT_3D('',#21966,#17580,#17581);
#15011=AXIS2_PLACEMENT_3D('',#21967,#17582,#17583);
#15012=AXIS2_PLACEMENT_3D('',#21968,#17584,#17585);
#15013=AXIS2_PLACEMENT_3D('',#21969,#17586,#17587);
#15014=AXIS2_PLACEMENT_3D('',#21971,#17588,#17589);
#15015=AXIS2_PLACEMENT_3D('',#21974,#17591,#17592);
#15016=AXIS2_PLACEMENT_3D('',#21975,#17593,#17594);
#15017=AXIS2_PLACEMENT_3D('',#21976,#17595,#17596);
#15018=AXIS2_PLACEMENT_3D('',#21977,#17597,#17598);
#15019=AXIS2_PLACEMENT_3D('',#21978,#17599,#17600);
#15020=AXIS2_PLACEMENT_3D('',#21980,#17601,#17602);
#15021=AXIS2_PLACEMENT_3D('',#21983,#17604,#17605);
#15022=AXIS2_PLACEMENT_3D('',#21984,#17606,#17607);
#15023=AXIS2_PLACEMENT_3D('',#21985,#17608,#17609);
#15024=AXIS2_PLACEMENT_3D('',#21986,#17610,#17611);
#15025=AXIS2_PLACEMENT_3D('',#21987,#17612,#17613);
#15026=AXIS2_PLACEMENT_3D('',#21989,#17614,#17615);
#15027=AXIS2_PLACEMENT_3D('',#21992,#17617,#17618);
#15028=AXIS2_PLACEMENT_3D('',#21993,#17619,#17620);
#15029=AXIS2_PLACEMENT_3D('',#21994,#17621,#17622);
#15030=AXIS2_PLACEMENT_3D('',#21996,#17623,#17624);
#15031=AXIS2_PLACEMENT_3D('',#21999,#17626,#17627);
#15032=AXIS2_PLACEMENT_3D('',#22000,#17628,#17629);
#15033=AXIS2_PLACEMENT_3D('',#22001,#17630,#17631);
#15034=AXIS2_PLACEMENT_3D('',#22003,#17632,#17633);
#15035=AXIS2_PLACEMENT_3D('',#22006,#17635,#17636);
#15036=AXIS2_PLACEMENT_3D('',#22007,#17637,#17638);
#15037=AXIS2_PLACEMENT_3D('',#22008,#17639,#17640);
#15038=AXIS2_PLACEMENT_3D('',#22009,#17641,#17642);
#15039=AXIS2_PLACEMENT_3D('',#22010,#17643,#17644);
#15040=AXIS2_PLACEMENT_3D('',#22012,#17645,#17646);
#15041=AXIS2_PLACEMENT_3D('',#22015,#17648,#17649);
#15042=AXIS2_PLACEMENT_3D('',#22016,#17650,#17651);
#15043=AXIS2_PLACEMENT_3D('',#22018,#17652,#17653);
#15044=AXIS2_PLACEMENT_3D('',#22021,#17655,#17656);
#15045=AXIS2_PLACEMENT_3D('',#22022,#17657,#17658);
#15046=AXIS2_PLACEMENT_3D('',#22023,#17659,#17660);
#15047=AXIS2_PLACEMENT_3D('',#22024,#17661,#17662);
#15048=AXIS2_PLACEMENT_3D('',#22025,#17663,#17664);
#15049=AXIS2_PLACEMENT_3D('',#22027,#17665,#17666);
#15050=AXIS2_PLACEMENT_3D('',#22030,#17668,#17669);
#15051=AXIS2_PLACEMENT_3D('',#22031,#17670,#17671);
#15052=AXIS2_PLACEMENT_3D('',#22033,#17672,#17673);
#15053=AXIS2_PLACEMENT_3D('',#22036,#17675,#17676);
#15054=AXIS2_PLACEMENT_3D('',#22037,#17677,#17678);
#15055=AXIS2_PLACEMENT_3D('',#22038,#17679,#17680);
#15056=AXIS2_PLACEMENT_3D('',#22039,#17681,#17682);
#15057=AXIS2_PLACEMENT_3D('',#22040,#17683,#17684);
#15058=AXIS2_PLACEMENT_3D('',#22042,#17685,#17686);
#15059=AXIS2_PLACEMENT_3D('',#22045,#17688,#17689);
#15060=AXIS2_PLACEMENT_3D('',#22046,#17690,#17691);
#15061=AXIS2_PLACEMENT_3D('',#22048,#17692,#17693);
#15062=AXIS2_PLACEMENT_3D('',#22051,#17695,#17696);
#15063=AXIS2_PLACEMENT_3D('',#22052,#17697,#17698);
#15064=AXIS2_PLACEMENT_3D('',#22053,#17699,#17700);
#15065=AXIS2_PLACEMENT_3D('',#22054,#17701,#17702);
#15066=AXIS2_PLACEMENT_3D('',#22055,#17703,#17704);
#15067=AXIS2_PLACEMENT_3D('',#22057,#17705,#17706);
#15068=AXIS2_PLACEMENT_3D('',#22060,#17708,#17709);
#15069=AXIS2_PLACEMENT_3D('',#22061,#17710,#17711);
#15070=AXIS2_PLACEMENT_3D('',#22063,#17712,#17713);
#15071=AXIS2_PLACEMENT_3D('',#22066,#17715,#17716);
#15072=AXIS2_PLACEMENT_3D('',#22067,#17717,#17718);
#15073=AXIS2_PLACEMENT_3D('',#22068,#17719,#17720);
#15074=AXIS2_PLACEMENT_3D('',#22069,#17721,#17722);
#15075=AXIS2_PLACEMENT_3D('',#22070,#17723,#17724);
#15076=AXIS2_PLACEMENT_3D('',#22072,#17725,#17726);
#15077=AXIS2_PLACEMENT_3D('',#22075,#17728,#17729);
#15078=AXIS2_PLACEMENT_3D('',#22076,#17730,#17731);
#15079=AXIS2_PLACEMENT_3D('',#22078,#17732,#17733);
#15080=AXIS2_PLACEMENT_3D('',#22081,#17735,#17736);
#15081=AXIS2_PLACEMENT_3D('',#22082,#17737,#17738);
#15082=AXIS2_PLACEMENT_3D('',#22083,#17739,#17740);
#15083=AXIS2_PLACEMENT_3D('',#22084,#17741,#17742);
#15084=AXIS2_PLACEMENT_3D('',#22085,#17743,#17744);
#15085=AXIS2_PLACEMENT_3D('',#22087,#17745,#17746);
#15086=AXIS2_PLACEMENT_3D('',#22090,#17748,#17749);
#15087=AXIS2_PLACEMENT_3D('',#22091,#17750,#17751);
#15088=AXIS2_PLACEMENT_3D('',#22093,#17752,#17753);
#15089=AXIS2_PLACEMENT_3D('',#22096,#17755,#17756);
#15090=AXIS2_PLACEMENT_3D('',#22097,#17757,#17758);
#15091=AXIS2_PLACEMENT_3D('',#22098,#17759,#17760);
#15092=AXIS2_PLACEMENT_3D('',#22099,#17761,#17762);
#15093=AXIS2_PLACEMENT_3D('',#22100,#17763,#17764);
#15094=AXIS2_PLACEMENT_3D('',#22102,#17765,#17766);
#15095=AXIS2_PLACEMENT_3D('',#22103,#17767,#17768);
#15096=AXIS2_PLACEMENT_3D('',#22105,#17769,#17770);
#15097=AXIS2_PLACEMENT_3D('',#22107,#17772,#17773);
#15098=AXIS2_PLACEMENT_3D('',#22109,#17774,#17775);
#15099=AXIS2_PLACEMENT_3D('',#22111,#17777,#17778);
#15100=AXIS2_PLACEMENT_3D('',#22113,#17779,#17780);
#15101=AXIS2_PLACEMENT_3D('',#22115,#17782,#17783);
#15102=AXIS2_PLACEMENT_3D('',#22117,#17784,#17785);
#15103=AXIS2_PLACEMENT_3D('',#22118,#17786,#17787);
#15104=AXIS2_PLACEMENT_3D('',#22120,#17788,#17789);
#15105=AXIS2_PLACEMENT_3D('',#22122,#17791,#17792);
#15106=AXIS2_PLACEMENT_3D('',#22124,#17793,#17794);
#15107=AXIS2_PLACEMENT_3D('',#22126,#17796,#17797);
#15108=AXIS2_PLACEMENT_3D('',#22128,#17798,#17799);
#15109=AXIS2_PLACEMENT_3D('',#22130,#17801,#17802);
#15110=AXIS2_PLACEMENT_3D('',#22131,#17803,#17804);
#15111=AXIS2_PLACEMENT_3D('',#22140,#17809,#17810);
#15112=AXIS2_PLACEMENT_3D('',#22146,#17814,#17815);
#15113=AXIS2_PLACEMENT_3D('',#22152,#17819,#17820);
#15114=AXIS2_PLACEMENT_3D('',#22158,#17824,#17825);
#15115=AXIS2_PLACEMENT_3D('',#22164,#17829,#17830);
#15116=AXIS2_PLACEMENT_3D('',#22167,#17833,#17834);
#15117=AXIS2_PLACEMENT_3D('',#22168,#17835,#17836);
#15118=AXIS2_PLACEMENT_3D('',#22169,#17837,#17838);
#15119=AXIS2_PLACEMENT_3D('',#22170,#17839,#17840);
#15120=AXIS2_PLACEMENT_3D('',#22171,#17841,#17842);
#15121=AXIS2_PLACEMENT_3D('',#22173,#17843,#17844);
#15122=AXIS2_PLACEMENT_3D('',#22176,#17846,#17847);
#15123=AXIS2_PLACEMENT_3D('',#22177,#17848,#17849);
#15124=AXIS2_PLACEMENT_3D('',#22179,#17850,#17851);
#15125=AXIS2_PLACEMENT_3D('',#22182,#17853,#17854);
#15126=AXIS2_PLACEMENT_3D('',#22183,#17855,#17856);
#15127=AXIS2_PLACEMENT_3D('',#22185,#17857,#17858);
#15128=AXIS2_PLACEMENT_3D('',#22188,#17860,#17861);
#15129=AXIS2_PLACEMENT_3D('',#22189,#17862,#17863);
#15130=AXIS2_PLACEMENT_3D('',#22198,#17868,#17869);
#15131=AXIS2_PLACEMENT_3D('',#22204,#17873,#17874);
#15132=AXIS2_PLACEMENT_3D('',#22210,#17878,#17879);
#15133=AXIS2_PLACEMENT_3D('',#22213,#17882,#17883);
#15134=AXIS2_PLACEMENT_3D('',#22214,#17884,#17885);
#15135=AXIS2_PLACEMENT_3D('',#22215,#17886,#17887);
#15136=AXIS2_PLACEMENT_3D('',#22216,#17888,#17889);
#15137=AXIS2_PLACEMENT_3D('',#22218,#17890,#17891);
#15138=AXIS2_PLACEMENT_3D('',#22221,#17893,#17894);
#15139=AXIS2_PLACEMENT_3D('',#22222,#17895,#17896);
#15140=AXIS2_PLACEMENT_3D('',#22224,#17897,#17898);
#15141=AXIS2_PLACEMENT_3D('',#22225,#17899,#17900);
#15142=AXIS2_PLACEMENT_3D('',#22227,#17901,#17902);
#15143=AXIS2_PLACEMENT_3D('',#22230,#17904,#17905);
#15144=AXIS2_PLACEMENT_3D('',#22231,#17906,#17907);
#15145=AXIS2_PLACEMENT_3D('',#22233,#17908,#17909);
#15146=AXIS2_PLACEMENT_3D('',#22234,#17910,#17911);
#15147=AXIS2_PLACEMENT_3D('',#22236,#17912,#17913);
#15148=AXIS2_PLACEMENT_3D('',#22239,#17915,#17916);
#15149=AXIS2_PLACEMENT_3D('',#22240,#17917,#17918);
#15150=AXIS2_PLACEMENT_3D('',#22242,#17919,#17920);
#15151=AXIS2_PLACEMENT_3D('',#22244,#17922,#17923);
#15152=AXIS2_PLACEMENT_3D('',#22246,#17924,#17925);
#15153=AXIS2_PLACEMENT_3D('',#22248,#17927,#17928);
#15154=AXIS2_PLACEMENT_3D('',#22257,#17933,#17934);
#15155=AXIS2_PLACEMENT_3D('',#22263,#17938,#17939);
#15156=AXIS2_PLACEMENT_3D('',#22269,#17943,#17944);
#15157=AXIS2_PLACEMENT_3D('',#22272,#17947,#17948);
#15158=AXIS2_PLACEMENT_3D('',#22273,#17949,#17950);
#15159=AXIS2_PLACEMENT_3D('',#22274,#17951,#17952);
#15160=AXIS2_PLACEMENT_3D('',#22275,#17953,#17954);
#15161=AXIS2_PLACEMENT_3D('',#22277,#17955,#17956);
#15162=AXIS2_PLACEMENT_3D('',#22280,#17958,#17959);
#15163=AXIS2_PLACEMENT_3D('',#22281,#17960,#17961);
#15164=AXIS2_PLACEMENT_3D('',#22283,#17962,#17963);
#15165=AXIS2_PLACEMENT_3D('',#22284,#17964,#17965);
#15166=AXIS2_PLACEMENT_3D('',#22286,#17966,#17967);
#15167=AXIS2_PLACEMENT_3D('',#22289,#17969,#17970);
#15168=AXIS2_PLACEMENT_3D('',#22290,#17971,#17972);
#15169=AXIS2_PLACEMENT_3D('',#22292,#17973,#17974);
#15170=AXIS2_PLACEMENT_3D('',#22293,#17975,#17976);
#15171=AXIS2_PLACEMENT_3D('',#22295,#17977,#17978);
#15172=AXIS2_PLACEMENT_3D('',#22298,#17980,#17981);
#15173=AXIS2_PLACEMENT_3D('',#22299,#17982,#17983);
#15174=AXIS2_PLACEMENT_3D('',#22302,#17985,#17986);
#15175=AXIS2_PLACEMENT_3D('',#22303,#17987,#17988);
#15176=AXIS2_PLACEMENT_3D('',#22306,#17990,#17991);
#15177=AXIS2_PLACEMENT_3D('',#22307,#17992,#17993);
#15178=AXIS2_PLACEMENT_3D('',#22316,#17998,#17999);
#15179=AXIS2_PLACEMENT_3D('',#22322,#18003,#18004);
#15180=AXIS2_PLACEMENT_3D('',#22328,#18008,#18009);
#15181=AXIS2_PLACEMENT_3D('',#22331,#18012,#18013);
#15182=AXIS2_PLACEMENT_3D('',#22332,#18014,#18015);
#15183=AXIS2_PLACEMENT_3D('',#22333,#18016,#18017);
#15184=AXIS2_PLACEMENT_3D('',#22334,#18018,#18019);
#15185=AXIS2_PLACEMENT_3D('',#22338,#18021,#18022);
#15186=AXIS2_PLACEMENT_3D('',#22339,#18023,#18024);
#15187=AXIS2_PLACEMENT_3D('',#22356,#18025,#18026);
#15188=AXIS2_PLACEMENT_3D('',#22359,#18028,#18029);
#15189=AXIS2_PLACEMENT_3D('',#22361,#18030,#18031);
#15190=AXIS2_PLACEMENT_3D('',#22376,#18032,#18033);
#15191=AXIS2_PLACEMENT_3D('',#22378,#18035,#18036);
#15192=AXIS2_PLACEMENT_3D('',#22380,#18037,#18038);
#15193=AXIS2_PLACEMENT_3D('',#22383,#18040,#18041);
#15194=AXIS2_PLACEMENT_3D('',#22384,#18042,#18043);
#15195=AXIS2_PLACEMENT_3D('',#22393,#18048,#18049);
#15196=AXIS2_PLACEMENT_3D('',#22399,#18053,#18054);
#15197=AXIS2_PLACEMENT_3D('',#22405,#18058,#18059);
#15198=AXIS2_PLACEMENT_3D('',#22408,#18062,#18063);
#15199=AXIS2_PLACEMENT_3D('',#22409,#18064,#18065);
#15200=AXIS2_PLACEMENT_3D('',#22410,#18066,#18067);
#15201=AXIS2_PLACEMENT_3D('',#22411,#18068,#18069);
#15202=AXIS2_PLACEMENT_3D('',#22413,#18070,#18071);
#15203=AXIS2_PLACEMENT_3D('',#22416,#18073,#18074);
#15204=AXIS2_PLACEMENT_3D('',#22417,#18075,#18076);
#15205=AXIS2_PLACEMENT_3D('',#22418,#18077,#18078);
#15206=AXIS2_PLACEMENT_3D('',#22420,#18079,#18080);
#15207=AXIS2_PLACEMENT_3D('',#22423,#18082,#18083);
#15208=AXIS2_PLACEMENT_3D('',#22424,#18084,#18085);
#15209=AXIS2_PLACEMENT_3D('',#22425,#18086,#18087);
#15210=AXIS2_PLACEMENT_3D('',#22427,#18088,#18089);
#15211=AXIS2_PLACEMENT_3D('',#22430,#18091,#18092);
#15212=AXIS2_PLACEMENT_3D('',#22431,#18093,#18094);
#15213=AXIS2_PLACEMENT_3D('',#22432,#18095,#18096);
#15214=AXIS2_PLACEMENT_3D('',#22433,#18097,#18098);
#15215=AXIS2_PLACEMENT_3D('',#22434,#18099,#18100);
#15216=AXIS2_PLACEMENT_3D('',#22436,#18101,#18102);
#15217=AXIS2_PLACEMENT_3D('',#22439,#18104,#18105);
#15218=AXIS2_PLACEMENT_3D('',#22440,#18106,#18107);
#15219=AXIS2_PLACEMENT_3D('',#22442,#18108,#18109);
#15220=AXIS2_PLACEMENT_3D('',#22445,#18111,#18112);
#15221=AXIS2_PLACEMENT_3D('',#22446,#18113,#18114);
#15222=AXIS2_PLACEMENT_3D('',#22447,#18115,#18116);
#15223=AXIS2_PLACEMENT_3D('',#22448,#18117,#18118);
#15224=AXIS2_PLACEMENT_3D('',#22449,#18119,#18120);
#15225=AXIS2_PLACEMENT_3D('',#22451,#18121,#18122);
#15226=AXIS2_PLACEMENT_3D('',#22454,#18124,#18125);
#15227=AXIS2_PLACEMENT_3D('',#22455,#18126,#18127);
#15228=AXIS2_PLACEMENT_3D('',#22457,#18128,#18129);
#15229=AXIS2_PLACEMENT_3D('',#22460,#18131,#18132);
#15230=AXIS2_PLACEMENT_3D('',#22461,#18133,#18134);
#15231=AXIS2_PLACEMENT_3D('',#22462,#18135,#18136);
#15232=AXIS2_PLACEMENT_3D('',#22463,#18137,#18138);
#15233=AXIS2_PLACEMENT_3D('',#22464,#18139,#18140);
#15234=AXIS2_PLACEMENT_3D('',#22466,#18141,#18142);
#15235=AXIS2_PLACEMENT_3D('',#22469,#18144,#18145);
#15236=AXIS2_PLACEMENT_3D('',#22470,#18146,#18147);
#15237=AXIS2_PLACEMENT_3D('',#22472,#18148,#18149);
#15238=AXIS2_PLACEMENT_3D('',#22475,#18151,#18152);
#15239=AXIS2_PLACEMENT_3D('',#22476,#18153,#18154);
#15240=AXIS2_PLACEMENT_3D('',#22477,#18155,#18156);
#15241=AXIS2_PLACEMENT_3D('',#22478,#18157,#18158);
#15242=AXIS2_PLACEMENT_3D('',#22479,#18159,#18160);
#15243=AXIS2_PLACEMENT_3D('',#22481,#18161,#18162);
#15244=AXIS2_PLACEMENT_3D('',#22484,#18164,#18165);
#15245=AXIS2_PLACEMENT_3D('',#22485,#18166,#18167);
#15246=AXIS2_PLACEMENT_3D('',#22487,#18168,#18169);
#15247=AXIS2_PLACEMENT_3D('',#22490,#18171,#18172);
#15248=AXIS2_PLACEMENT_3D('',#22491,#18173,#18174);
#15249=AXIS2_PLACEMENT_3D('',#22492,#18175,#18176);
#15250=AXIS2_PLACEMENT_3D('',#22493,#18177,#18178);
#15251=AXIS2_PLACEMENT_3D('',#22494,#18179,#18180);
#15252=AXIS2_PLACEMENT_3D('',#22496,#18181,#18182);
#15253=AXIS2_PLACEMENT_3D('',#22499,#18184,#18185);
#15254=AXIS2_PLACEMENT_3D('',#22500,#18186,#18187);
#15255=AXIS2_PLACEMENT_3D('',#22502,#18188,#18189);
#15256=AXIS2_PLACEMENT_3D('',#22505,#18191,#18192);
#15257=AXIS2_PLACEMENT_3D('',#22506,#18193,#18194);
#15258=AXIS2_PLACEMENT_3D('',#22507,#18195,#18196);
#15259=AXIS2_PLACEMENT_3D('',#22508,#18197,#18198);
#15260=AXIS2_PLACEMENT_3D('',#22509,#18199,#18200);
#15261=AXIS2_PLACEMENT_3D('',#22511,#18201,#18202);
#15262=AXIS2_PLACEMENT_3D('',#22514,#18204,#18205);
#15263=AXIS2_PLACEMENT_3D('',#22515,#18206,#18207);
#15264=AXIS2_PLACEMENT_3D('',#22517,#18208,#18209);
#15265=AXIS2_PLACEMENT_3D('',#22520,#18211,#18212);
#15266=AXIS2_PLACEMENT_3D('',#22521,#18213,#18214);
#15267=AXIS2_PLACEMENT_3D('',#22522,#18215,#18216);
#15268=AXIS2_PLACEMENT_3D('',#22523,#18217,#18218);
#15269=AXIS2_PLACEMENT_3D('',#22524,#18219,#18220);
#15270=AXIS2_PLACEMENT_3D('',#22525,#18221,#18222);
#15271=AXIS2_PLACEMENT_3D('',#22527,#18223,#18224);
#15272=AXIS2_PLACEMENT_3D('',#22530,#18226,#18227);
#15273=AXIS2_PLACEMENT_3D('',#22531,#18228,#18229);
#15274=AXIS2_PLACEMENT_3D('',#22533,#18230,#18231);
#15275=AXIS2_PLACEMENT_3D('',#22536,#18233,#18234);
#15276=AXIS2_PLACEMENT_3D('',#22537,#18235,#18236);
#15277=AXIS2_PLACEMENT_3D('',#22539,#18237,#18238);
#15278=AXIS2_PLACEMENT_3D('',#22542,#18240,#18241);
#15279=AXIS2_PLACEMENT_3D('',#22543,#18242,#18243);
#15280=AXIS2_PLACEMENT_3D('',#22552,#18248,#18249);
#15281=AXIS2_PLACEMENT_3D('',#22558,#18253,#18254);
#15282=AXIS2_PLACEMENT_3D('',#22564,#18258,#18259);
#15283=AXIS2_PLACEMENT_3D('',#22567,#18262,#18263);
#15284=AXIS2_PLACEMENT_3D('',#22568,#18264,#18265);
#15285=AXIS2_PLACEMENT_3D('',#22569,#18266,#18267);
#15286=AXIS2_PLACEMENT_3D('',#22570,#18268,#18269);
#15287=AXIS2_PLACEMENT_3D('',#22572,#18270,#18271);
#15288=AXIS2_PLACEMENT_3D('',#22575,#18273,#18274);
#15289=AXIS2_PLACEMENT_3D('',#22576,#18275,#18276);
#15290=AXIS2_PLACEMENT_3D('',#22578,#18277,#18278);
#15291=AXIS2_PLACEMENT_3D('',#22579,#18279,#18280);
#15292=AXIS2_PLACEMENT_3D('',#22581,#18281,#18282);
#15293=AXIS2_PLACEMENT_3D('',#22584,#18284,#18285);
#15294=AXIS2_PLACEMENT_3D('',#22585,#18286,#18287);
#15295=AXIS2_PLACEMENT_3D('',#22587,#18288,#18289);
#15296=AXIS2_PLACEMENT_3D('',#22588,#18290,#18291);
#15297=AXIS2_PLACEMENT_3D('',#22590,#18292,#18293);
#15298=AXIS2_PLACEMENT_3D('',#22593,#18295,#18296);
#15299=AXIS2_PLACEMENT_3D('',#22594,#18297,#18298);
#15300=AXIS2_PLACEMENT_3D('',#22596,#18299,#18300);
#15301=AXIS2_PLACEMENT_3D('',#22598,#18302,#18303);
#15302=AXIS2_PLACEMENT_3D('',#22600,#18304,#18305);
#15303=AXIS2_PLACEMENT_3D('',#22602,#18307,#18308);
#15304=AXIS2_PLACEMENT_3D('',#22611,#18313,#18314);
#15305=AXIS2_PLACEMENT_3D('',#22617,#18318,#18319);
#15306=AXIS2_PLACEMENT_3D('',#22623,#18323,#18324);
#15307=AXIS2_PLACEMENT_3D('',#22626,#18327,#18328);
#15308=AXIS2_PLACEMENT_3D('',#22627,#18329,#18330);
#15309=AXIS2_PLACEMENT_3D('',#22628,#18331,#18332);
#15310=AXIS2_PLACEMENT_3D('',#22629,#18333,#18334);
#15311=AXIS2_PLACEMENT_3D('',#22631,#18335,#18336);
#15312=AXIS2_PLACEMENT_3D('',#22634,#18338,#18339);
#15313=AXIS2_PLACEMENT_3D('',#22635,#18340,#18341);
#15314=AXIS2_PLACEMENT_3D('',#22637,#18342,#18343);
#15315=AXIS2_PLACEMENT_3D('',#22638,#18344,#18345);
#15316=AXIS2_PLACEMENT_3D('',#22640,#18346,#18347);
#15317=AXIS2_PLACEMENT_3D('',#22643,#18349,#18350);
#15318=AXIS2_PLACEMENT_3D('',#22644,#18351,#18352);
#15319=AXIS2_PLACEMENT_3D('',#22646,#18353,#18354);
#15320=AXIS2_PLACEMENT_3D('',#22647,#18355,#18356);
#15321=AXIS2_PLACEMENT_3D('',#22649,#18357,#18358);
#15322=AXIS2_PLACEMENT_3D('',#22652,#18360,#18361);
#15323=AXIS2_PLACEMENT_3D('',#22653,#18362,#18363);
#15324=AXIS2_PLACEMENT_3D('',#22656,#18365,#18366);
#15325=AXIS2_PLACEMENT_3D('',#22657,#18367,#18368);
#15326=AXIS2_PLACEMENT_3D('',#22660,#18370,#18371);
#15327=AXIS2_PLACEMENT_3D('',#22661,#18372,#18373);
#15328=AXIS2_PLACEMENT_3D('',#22670,#18378,#18379);
#15329=AXIS2_PLACEMENT_3D('',#22676,#18383,#18384);
#15330=AXIS2_PLACEMENT_3D('',#22682,#18388,#18389);
#15331=AXIS2_PLACEMENT_3D('',#22685,#18392,#18393);
#15332=AXIS2_PLACEMENT_3D('',#22686,#18394,#18395);
#15333=AXIS2_PLACEMENT_3D('',#22687,#18396,#18397);
#15334=AXIS2_PLACEMENT_3D('',#22688,#18398,#18399);
#15335=AXIS2_PLACEMENT_3D('',#22692,#18401,#18402);
#15336=AXIS2_PLACEMENT_3D('',#22693,#18403,#18404);
#15337=AXIS2_PLACEMENT_3D('',#22710,#18405,#18406);
#15338=AXIS2_PLACEMENT_3D('',#22713,#18408,#18409);
#15339=AXIS2_PLACEMENT_3D('',#22715,#18410,#18411);
#15340=AXIS2_PLACEMENT_3D('',#22730,#18412,#18413);
#15341=AXIS2_PLACEMENT_3D('',#22732,#18415,#18416);
#15342=AXIS2_PLACEMENT_3D('',#22734,#18417,#18418);
#15343=AXIS2_PLACEMENT_3D('',#22737,#18420,#18421);
#15344=AXIS2_PLACEMENT_3D('',#22738,#18422,#18423);
#15345=AXIS2_PLACEMENT_3D('',#22747,#18428,#18429);
#15346=AXIS2_PLACEMENT_3D('',#22753,#18433,#18434);
#15347=AXIS2_PLACEMENT_3D('',#22759,#18438,#18439);
#15348=AXIS2_PLACEMENT_3D('',#22762,#18442,#18443);
#15349=AXIS2_PLACEMENT_3D('',#22763,#18444,#18445);
#15350=AXIS2_PLACEMENT_3D('',#22764,#18446,#18447);
#15351=AXIS2_PLACEMENT_3D('',#22765,#18448,#18449);
#15352=AXIS2_PLACEMENT_3D('',#22767,#18450,#18451);
#15353=AXIS2_PLACEMENT_3D('',#22770,#18453,#18454);
#15354=AXIS2_PLACEMENT_3D('',#22771,#18455,#18456);
#15355=AXIS2_PLACEMENT_3D('',#22772,#18457,#18458);
#15356=AXIS2_PLACEMENT_3D('',#22774,#18459,#18460);
#15357=AXIS2_PLACEMENT_3D('',#22777,#18462,#18463);
#15358=AXIS2_PLACEMENT_3D('',#22778,#18464,#18465);
#15359=AXIS2_PLACEMENT_3D('',#22779,#18466,#18467);
#15360=AXIS2_PLACEMENT_3D('',#22781,#18468,#18469);
#15361=AXIS2_PLACEMENT_3D('',#22784,#18471,#18472);
#15362=AXIS2_PLACEMENT_3D('',#22785,#18473,#18474);
#15363=AXIS2_PLACEMENT_3D('',#22786,#18475,#18476);
#15364=AXIS2_PLACEMENT_3D('',#22787,#18477,#18478);
#15365=AXIS2_PLACEMENT_3D('',#22788,#18479,#18480);
#15366=AXIS2_PLACEMENT_3D('',#22790,#18481,#18482);
#15367=AXIS2_PLACEMENT_3D('',#22793,#18484,#18485);
#15368=AXIS2_PLACEMENT_3D('',#22794,#18486,#18487);
#15369=AXIS2_PLACEMENT_3D('',#22796,#18488,#18489);
#15370=AXIS2_PLACEMENT_3D('',#22799,#18491,#18492);
#15371=AXIS2_PLACEMENT_3D('',#22800,#18493,#18494);
#15372=AXIS2_PLACEMENT_3D('',#22801,#18495,#18496);
#15373=AXIS2_PLACEMENT_3D('',#22802,#18497,#18498);
#15374=AXIS2_PLACEMENT_3D('',#22803,#18499,#18500);
#15375=AXIS2_PLACEMENT_3D('',#22805,#18501,#18502);
#15376=AXIS2_PLACEMENT_3D('',#22808,#18504,#18505);
#15377=AXIS2_PLACEMENT_3D('',#22809,#18506,#18507);
#15378=AXIS2_PLACEMENT_3D('',#22811,#18508,#18509);
#15379=AXIS2_PLACEMENT_3D('',#22814,#18511,#18512);
#15380=AXIS2_PLACEMENT_3D('',#22815,#18513,#18514);
#15381=AXIS2_PLACEMENT_3D('',#22816,#18515,#18516);
#15382=AXIS2_PLACEMENT_3D('',#22817,#18517,#18518);
#15383=AXIS2_PLACEMENT_3D('',#22818,#18519,#18520);
#15384=AXIS2_PLACEMENT_3D('',#22820,#18521,#18522);
#15385=AXIS2_PLACEMENT_3D('',#22823,#18524,#18525);
#15386=AXIS2_PLACEMENT_3D('',#22824,#18526,#18527);
#15387=AXIS2_PLACEMENT_3D('',#22826,#18528,#18529);
#15388=AXIS2_PLACEMENT_3D('',#22829,#18531,#18532);
#15389=AXIS2_PLACEMENT_3D('',#22830,#18533,#18534);
#15390=AXIS2_PLACEMENT_3D('',#22831,#18535,#18536);
#15391=AXIS2_PLACEMENT_3D('',#22832,#18537,#18538);
#15392=AXIS2_PLACEMENT_3D('',#22833,#18539,#18540);
#15393=AXIS2_PLACEMENT_3D('',#22835,#18541,#18542);
#15394=AXIS2_PLACEMENT_3D('',#22838,#18544,#18545);
#15395=AXIS2_PLACEMENT_3D('',#22839,#18546,#18547);
#15396=AXIS2_PLACEMENT_3D('',#22841,#18548,#18549);
#15397=AXIS2_PLACEMENT_3D('',#22844,#18551,#18552);
#15398=AXIS2_PLACEMENT_3D('',#22845,#18553,#18554);
#15399=AXIS2_PLACEMENT_3D('',#22846,#18555,#18556);
#15400=AXIS2_PLACEMENT_3D('',#22847,#18557,#18558);
#15401=AXIS2_PLACEMENT_3D('',#22848,#18559,#18560);
#15402=AXIS2_PLACEMENT_3D('',#22850,#18561,#18562);
#15403=AXIS2_PLACEMENT_3D('',#22853,#18564,#18565);
#15404=AXIS2_PLACEMENT_3D('',#22854,#18566,#18567);
#15405=AXIS2_PLACEMENT_3D('',#22856,#18568,#18569);
#15406=AXIS2_PLACEMENT_3D('',#22859,#18571,#18572);
#15407=AXIS2_PLACEMENT_3D('',#22860,#18573,#18574);
#15408=AXIS2_PLACEMENT_3D('',#22861,#18575,#18576);
#15409=AXIS2_PLACEMENT_3D('',#22862,#18577,#18578);
#15410=AXIS2_PLACEMENT_3D('',#22863,#18579,#18580);
#15411=AXIS2_PLACEMENT_3D('',#22865,#18581,#18582);
#15412=AXIS2_PLACEMENT_3D('',#22868,#18584,#18585);
#15413=AXIS2_PLACEMENT_3D('',#22869,#18586,#18587);
#15414=AXIS2_PLACEMENT_3D('',#22871,#18588,#18589);
#15415=AXIS2_PLACEMENT_3D('',#22874,#18591,#18592);
#15416=AXIS2_PLACEMENT_3D('',#22875,#18593,#18594);
#15417=AXIS2_PLACEMENT_3D('',#22876,#18595,#18596);
#15418=AXIS2_PLACEMENT_3D('',#22877,#18597,#18598);
#15419=AXIS2_PLACEMENT_3D('',#22878,#18599,#18600);
#15420=AXIS2_PLACEMENT_3D('',#22879,#18601,#18602);
#15421=AXIS2_PLACEMENT_3D('',#22882,#18603,#18604);
#15422=AXIS2_PLACEMENT_3D('',#22888,#18608,#18609);
#15423=AXIS2_PLACEMENT_3D('',#22894,#18613,#18614);
#15424=AXIS2_PLACEMENT_3D('',#22896,#18615,#18616);
#15425=AXIS2_PLACEMENT_3D('',#22900,#18619,#18620);
#15426=AXIS2_PLACEMENT_3D('',#22903,#18623,#18624);
#15427=AXIS2_PLACEMENT_3D('',#22904,#18625,#18626);
#15428=AXIS2_PLACEMENT_3D('',#22906,#18627,#18628);
#15429=AXIS2_PLACEMENT_3D('',#22908,#18629,#18630);
#15430=AXIS2_PLACEMENT_3D('',#22909,#18631,#18632);
#15431=AXIS2_PLACEMENT_3D('',#22911,#18633,#18634);
#15432=AXIS2_PLACEMENT_3D('',#22913,#18636,#18637);
#15433=AXIS2_PLACEMENT_3D('',#22915,#18638,#18639);
#15434=AXIS2_PLACEMENT_3D('',#22916,#18640,#18641);
#15435=AXIS2_PLACEMENT_3D('',#22918,#18642,#18643);
#15436=AXIS2_PLACEMENT_3D('',#22920,#18645,#18646);
#15437=AXIS2_PLACEMENT_3D('',#22922,#18647,#18648);
#15438=AXIS2_PLACEMENT_3D('',#22923,#18649,#18650);
#15439=AXIS2_PLACEMENT_3D('',#22925,#18651,#18652);
#15440=AXIS2_PLACEMENT_3D('',#22927,#18654,#18655);
#15441=AXIS2_PLACEMENT_3D('',#22929,#18656,#18657);
#15442=AXIS2_PLACEMENT_3D('',#22930,#18658,#18659);
#15443=AXIS2_PLACEMENT_3D('',#22932,#18660,#18661);
#15444=AXIS2_PLACEMENT_3D('',#22934,#18663,#18664);
#15445=AXIS2_PLACEMENT_3D('',#22936,#18665,#18666);
#15446=AXIS2_PLACEMENT_3D('',#22937,#18667,#18668);
#15447=AXIS2_PLACEMENT_3D('',#22939,#18669,#18670);
#15448=AXIS2_PLACEMENT_3D('',#22941,#18672,#18673);
#15449=AXIS2_PLACEMENT_3D('',#22943,#18674,#18675);
#15450=AXIS2_PLACEMENT_3D('',#22944,#18676,#18677);
#15451=AXIS2_PLACEMENT_3D('',#22946,#18679,#18680);
#15452=AXIS2_PLACEMENT_3D('',#22947,#18681,#18682);
#15453=AXIS2_PLACEMENT_3D('',#22950,#18683,#18684);
#15454=AXIS2_PLACEMENT_3D('',#22954,#18686,#18687);
#15455=AXIS2_PLACEMENT_3D('',#22956,#18689,#18690);
#15456=AXIS2_PLACEMENT_3D('',#22962,#18694,#18695);
#15457=AXIS2_PLACEMENT_3D('',#22964,#18696,#18697);
#15458=AXIS2_PLACEMENT_3D('',#22966,#18698,#18699);
#15459=AXIS2_PLACEMENT_3D('',#22968,#18701,#18702);
#15460=AXIS2_PLACEMENT_3D('',#22971,#18705,#18706);
#15461=AXIS2_PLACEMENT_3D('',#22973,#18707,#18708);
#15462=AXIS2_PLACEMENT_3D('',#22975,#18709,#18710);
#15463=AXIS2_PLACEMENT_3D('',#22976,#18711,#18712);
#15464=AXIS2_PLACEMENT_3D('',#22978,#18713,#18714);
#15465=AXIS2_PLACEMENT_3D('',#22980,#18716,#18717);
#15466=AXIS2_PLACEMENT_3D('',#22982,#18718,#18719);
#15467=AXIS2_PLACEMENT_3D('',#22983,#18720,#18721);
#15468=AXIS2_PLACEMENT_3D('',#22985,#18723,#18724);
#15469=AXIS2_PLACEMENT_3D('',#22986,#18725,#18726);
#15470=AXIS2_PLACEMENT_3D('',#22987,#18727,#18728);
#15471=AXIS2_PLACEMENT_3D('',#22988,#18729,#18730);
#15472=AXIS2_PLACEMENT_3D('',#22990,#18731,#18732);
#15473=AXIS2_PLACEMENT_3D('',#22991,#18733,#18734);
#15474=AXIS2_PLACEMENT_3D('',#23000,#18739,#18740);
#15475=AXIS2_PLACEMENT_3D('',#23006,#18744,#18745);
#15476=AXIS2_PLACEMENT_3D('',#23012,#18749,#18750);
#15477=AXIS2_PLACEMENT_3D('',#23018,#18754,#18755);
#15478=AXIS2_PLACEMENT_3D('',#23024,#18759,#18760);
#15479=AXIS2_PLACEMENT_3D('',#23027,#18763,#18764);
#15480=AXIS2_PLACEMENT_3D('',#23028,#18765,#18766);
#15481=AXIS2_PLACEMENT_3D('',#23030,#18767,#18768);
#15482=AXIS2_PLACEMENT_3D('',#23031,#18769,#18770);
#15483=AXIS2_PLACEMENT_3D('',#23033,#18771,#18772);
#15484=AXIS2_PLACEMENT_3D('',#23035,#18774,#18775);
#15485=AXIS2_PLACEMENT_3D('',#23037,#18777,#18778);
#15486=AXIS2_PLACEMENT_3D('',#23038,#18779,#18780);
#15487=AXIS2_PLACEMENT_3D('',#23039,#18781,#18782);
#15488=AXIS2_PLACEMENT_3D('',#23041,#18783,#18784);
#15489=AXIS2_PLACEMENT_3D('',#23044,#18786,#18787);
#15490=AXIS2_PLACEMENT_3D('',#23045,#18788,#18789);
#15491=AXIS2_PLACEMENT_3D('',#23050,#18791,#18792);
#15492=AXIS2_PLACEMENT_3D('',#23053,#18794,#18795);
#15493=AXIS2_PLACEMENT_3D('',#23054,#18796,#18797);
#15494=AXIS2_PLACEMENT_3D('',#23059,#18799,#18800);
#15495=AXIS2_PLACEMENT_3D('',#23062,#18802,#18803);
#15496=AXIS2_PLACEMENT_3D('',#23063,#18804,#18805);
#15497=AXIS2_PLACEMENT_3D('',#23069,#18809,#18810);
#15498=AXIS2_PLACEMENT_3D('',#23075,#18814,#18815);
#15499=AXIS2_PLACEMENT_3D('',#23081,#18819,#18820);
#15500=AXIS2_PLACEMENT_3D('',#23083,#18821,#18822);
#15501=AXIS2_PLACEMENT_3D('',#23086,#18824,#18825);
#15502=AXIS2_PLACEMENT_3D('',#23087,#18826,#18827);
#15503=AXIS2_PLACEMENT_3D('',#23088,#18828,#18829);
#15504=AXIS2_PLACEMENT_3D('',#23089,#18830,#18831);
#15505=AXIS2_PLACEMENT_3D('',#23090,#18832,#18833);
#15506=AXIS2_PLACEMENT_3D('',#23093,#18835,#18836);
#15507=AXIS2_PLACEMENT_3D('',#23095,#18837,#18838);
#15508=AXIS2_PLACEMENT_3D('',#23096,#18839,#18840);
#15509=AXIS2_PLACEMENT_3D('',#23100,#18843,#18844);
#15510=AXIS2_PLACEMENT_3D('',#23103,#18846,#18847);
#15511=AXIS2_PLACEMENT_3D('',#23104,#18848,#18849);
#15512=AXIS2_PLACEMENT_3D('',#23105,#18850,#18851);
#15513=AXIS2_PLACEMENT_3D('',#23106,#18852,#18853);
#15514=AXIS2_PLACEMENT_3D('',#23107,#18854,#18855);
#15515=AXIS2_PLACEMENT_3D('',#23108,#18856,#18857);
#15516=AXIS2_PLACEMENT_3D('',#23110,#18858,#18859);
#15517=AXIS2_PLACEMENT_3D('',#23113,#18861,#18862);
#15518=AXIS2_PLACEMENT_3D('',#23114,#18863,#18864);
#15519=AXIS2_PLACEMENT_3D('',#23116,#18865,#18866);
#15520=AXIS2_PLACEMENT_3D('',#23119,#18868,#18869);
#15521=AXIS2_PLACEMENT_3D('',#23120,#18870,#18871);
#15522=AXIS2_PLACEMENT_3D('',#23121,#18872,#18873);
#15523=AXIS2_PLACEMENT_3D('',#23122,#18874,#18875);
#15524=AXIS2_PLACEMENT_3D('',#23123,#18876,#18877);
#15525=AXIS2_PLACEMENT_3D('',#23125,#18878,#18879);
#15526=AXIS2_PLACEMENT_3D('',#23128,#18881,#18882);
#15527=AXIS2_PLACEMENT_3D('',#23129,#18883,#18884);
#15528=AXIS2_PLACEMENT_3D('',#23131,#18885,#18886);
#15529=AXIS2_PLACEMENT_3D('',#23134,#18888,#18889);
#15530=AXIS2_PLACEMENT_3D('',#23135,#18890,#18891);
#15531=AXIS2_PLACEMENT_3D('',#23136,#18892,#18893);
#15532=AXIS2_PLACEMENT_3D('',#23137,#18894,#18895);
#15533=AXIS2_PLACEMENT_3D('',#23138,#18896,#18897);
#15534=AXIS2_PLACEMENT_3D('',#23140,#18898,#18899);
#15535=AXIS2_PLACEMENT_3D('',#23143,#18901,#18902);
#15536=AXIS2_PLACEMENT_3D('',#23144,#18903,#18904);
#15537=AXIS2_PLACEMENT_3D('',#23146,#18905,#18906);
#15538=AXIS2_PLACEMENT_3D('',#23149,#18908,#18909);
#15539=AXIS2_PLACEMENT_3D('',#23150,#18910,#18911);
#15540=AXIS2_PLACEMENT_3D('',#23151,#18912,#18913);
#15541=AXIS2_PLACEMENT_3D('',#23152,#18914,#18915);
#15542=AXIS2_PLACEMENT_3D('',#23153,#18916,#18917);
#15543=AXIS2_PLACEMENT_3D('',#23155,#18918,#18919);
#15544=AXIS2_PLACEMENT_3D('',#23158,#18921,#18922);
#15545=AXIS2_PLACEMENT_3D('',#23159,#18923,#18924);
#15546=AXIS2_PLACEMENT_3D('',#23164,#18926,#18927);
#15547=AXIS2_PLACEMENT_3D('',#23167,#18929,#18930);
#15548=AXIS2_PLACEMENT_3D('',#23168,#18931,#18932);
#15549=AXIS2_PLACEMENT_3D('',#23173,#18934,#18935);
#15550=AXIS2_PLACEMENT_3D('',#23176,#18937,#18938);
#15551=AXIS2_PLACEMENT_3D('',#23177,#18939,#18940);
#15552=AXIS2_PLACEMENT_3D('',#23183,#18944,#18945);
#15553=AXIS2_PLACEMENT_3D('',#23189,#18949,#18950);
#15554=AXIS2_PLACEMENT_3D('',#23195,#18954,#18955);
#15555=AXIS2_PLACEMENT_3D('',#23197,#18956,#18957);
#15556=AXIS2_PLACEMENT_3D('',#23200,#18959,#18960);
#15557=AXIS2_PLACEMENT_3D('',#23201,#18961,#18962);
#15558=AXIS2_PLACEMENT_3D('',#23202,#18963,#18964);
#15559=AXIS2_PLACEMENT_3D('',#23203,#18965,#18966);
#15560=AXIS2_PLACEMENT_3D('',#23204,#18967,#18968);
#15561=AXIS2_PLACEMENT_3D('',#23207,#18970,#18971);
#15562=AXIS2_PLACEMENT_3D('',#23209,#18972,#18973);
#15563=AXIS2_PLACEMENT_3D('',#23210,#18974,#18975);
#15564=AXIS2_PLACEMENT_3D('',#23214,#18978,#18979);
#15565=AXIS2_PLACEMENT_3D('',#23217,#18981,#18982);
#15566=AXIS2_PLACEMENT_3D('',#23218,#18983,#18984);
#15567=AXIS2_PLACEMENT_3D('',#23219,#18985,#18986);
#15568=AXIS2_PLACEMENT_3D('',#23220,#18987,#18988);
#15569=AXIS2_PLACEMENT_3D('',#23221,#18989,#18990);
#15570=AXIS2_PLACEMENT_3D('',#23222,#18991,#18992);
#15571=AXIS2_PLACEMENT_3D('',#23224,#18993,#18994);
#15572=AXIS2_PLACEMENT_3D('',#23227,#18996,#18997);
#15573=AXIS2_PLACEMENT_3D('',#23228,#18998,#18999);
#15574=AXIS2_PLACEMENT_3D('',#23230,#19000,#19001);
#15575=AXIS2_PLACEMENT_3D('',#23233,#19003,#19004);
#15576=AXIS2_PLACEMENT_3D('',#23234,#19005,#19006);
#15577=AXIS2_PLACEMENT_3D('',#23235,#19007,#19008);
#15578=AXIS2_PLACEMENT_3D('',#23236,#19009,#19010);
#15579=AXIS2_PLACEMENT_3D('',#23237,#19011,#19012);
#15580=AXIS2_PLACEMENT_3D('',#23239,#19013,#19014);
#15581=AXIS2_PLACEMENT_3D('',#23242,#19016,#19017);
#15582=AXIS2_PLACEMENT_3D('',#23243,#19018,#19019);
#15583=AXIS2_PLACEMENT_3D('',#23245,#19020,#19021);
#15584=AXIS2_PLACEMENT_3D('',#23248,#19023,#19024);
#15585=AXIS2_PLACEMENT_3D('',#23249,#19025,#19026);
#15586=AXIS2_PLACEMENT_3D('',#23250,#19027,#19028);
#15587=AXIS2_PLACEMENT_3D('',#23251,#19029,#19030);
#15588=AXIS2_PLACEMENT_3D('',#23252,#19031,#19032);
#15589=AXIS2_PLACEMENT_3D('',#23254,#19033,#19034);
#15590=AXIS2_PLACEMENT_3D('',#23257,#19036,#19037);
#15591=AXIS2_PLACEMENT_3D('',#23258,#19038,#19039);
#15592=AXIS2_PLACEMENT_3D('',#23260,#19040,#19041);
#15593=AXIS2_PLACEMENT_3D('',#23263,#19043,#19044);
#15594=AXIS2_PLACEMENT_3D('',#23264,#19045,#19046);
#15595=AXIS2_PLACEMENT_3D('',#23265,#19047,#19048);
#15596=AXIS2_PLACEMENT_3D('',#23266,#19049,#19050);
#15597=AXIS2_PLACEMENT_3D('',#23267,#19051,#19052);
#15598=AXIS2_PLACEMENT_3D('',#23269,#19053,#19054);
#15599=AXIS2_PLACEMENT_3D('',#23272,#19056,#19057);
#15600=AXIS2_PLACEMENT_3D('',#23273,#19058,#19059);
#15601=AXIS2_PLACEMENT_3D('',#23274,#19060,#19061);
#15602=AXIS2_PLACEMENT_3D('',#23276,#19062,#19063);
#15603=AXIS2_PLACEMENT_3D('',#23279,#19065,#19066);
#15604=AXIS2_PLACEMENT_3D('',#23280,#19067,#19068);
#15605=AXIS2_PLACEMENT_3D('',#23281,#19069,#19070);
#15606=AXIS2_PLACEMENT_3D('',#23283,#19071,#19072);
#15607=AXIS2_PLACEMENT_3D('',#23286,#19074,#19075);
#15608=AXIS2_PLACEMENT_3D('',#23287,#19076,#19077);
#15609=AXIS2_PLACEMENT_3D('',#23288,#19078,#19079);
#15610=AXIS2_PLACEMENT_3D('',#23289,#19080,#19081);
#15611=AXIS2_PLACEMENT_3D('',#23290,#19082,#19083);
#15612=AXIS2_PLACEMENT_3D('',#23292,#19084,#19085);
#15613=AXIS2_PLACEMENT_3D('',#23295,#19087,#19088);
#15614=AXIS2_PLACEMENT_3D('',#23296,#19089,#19090);
#15615=AXIS2_PLACEMENT_3D('',#23298,#19091,#19092);
#15616=AXIS2_PLACEMENT_3D('',#23301,#19094,#19095);
#15617=AXIS2_PLACEMENT_3D('',#23302,#19096,#19097);
#15618=AXIS2_PLACEMENT_3D('',#23303,#19098,#19099);
#15619=AXIS2_PLACEMENT_3D('',#23304,#19100,#19101);
#15620=AXIS2_PLACEMENT_3D('',#23305,#19102,#19103);
#15621=AXIS2_PLACEMENT_3D('',#23307,#19104,#19105);
#15622=AXIS2_PLACEMENT_3D('',#23310,#19107,#19108);
#15623=AXIS2_PLACEMENT_3D('',#23311,#19109,#19110);
#15624=AXIS2_PLACEMENT_3D('',#23313,#19111,#19112);
#15625=AXIS2_PLACEMENT_3D('',#23316,#19114,#19115);
#15626=AXIS2_PLACEMENT_3D('',#23317,#19116,#19117);
#15627=AXIS2_PLACEMENT_3D('',#23318,#19118,#19119);
#15628=AXIS2_PLACEMENT_3D('',#23319,#19120,#19121);
#15629=AXIS2_PLACEMENT_3D('',#23320,#19122,#19123);
#15630=AXIS2_PLACEMENT_3D('',#23322,#19124,#19125);
#15631=AXIS2_PLACEMENT_3D('',#23325,#19127,#19128);
#15632=AXIS2_PLACEMENT_3D('',#23326,#19129,#19130);
#15633=AXIS2_PLACEMENT_3D('',#23328,#19131,#19132);
#15634=AXIS2_PLACEMENT_3D('',#23331,#19134,#19135);
#15635=AXIS2_PLACEMENT_3D('',#23332,#19136,#19137);
#15636=AXIS2_PLACEMENT_3D('',#23333,#19138,#19139);
#15637=AXIS2_PLACEMENT_3D('',#23334,#19140,#19141);
#15638=AXIS2_PLACEMENT_3D('',#23335,#19142,#19143);
#15639=AXIS2_PLACEMENT_3D('',#23337,#19144,#19145);
#15640=AXIS2_PLACEMENT_3D('',#23340,#19147,#19148);
#15641=AXIS2_PLACEMENT_3D('',#23341,#19149,#19150);
#15642=AXIS2_PLACEMENT_3D('',#23343,#19151,#19152);
#15643=AXIS2_PLACEMENT_3D('',#23346,#19154,#19155);
#15644=AXIS2_PLACEMENT_3D('',#23347,#19156,#19157);
#15645=AXIS2_PLACEMENT_3D('',#23348,#19158,#19159);
#15646=AXIS2_PLACEMENT_3D('',#23349,#19160,#19161);
#15647=AXIS2_PLACEMENT_3D('',#23350,#19162,#19163);
#15648=AXIS2_PLACEMENT_3D('',#23352,#19164,#19165);
#15649=AXIS2_PLACEMENT_3D('',#23355,#19167,#19168);
#15650=AXIS2_PLACEMENT_3D('',#23356,#19169,#19170);
#15651=AXIS2_PLACEMENT_3D('',#23358,#19171,#19172);
#15652=AXIS2_PLACEMENT_3D('',#23361,#19174,#19175);
#15653=AXIS2_PLACEMENT_3D('',#23362,#19176,#19177);
#15654=AXIS2_PLACEMENT_3D('',#23363,#19178,#19179);
#15655=AXIS2_PLACEMENT_3D('',#23364,#19180,#19181);
#15656=AXIS2_PLACEMENT_3D('',#23365,#19182,#19183);
#15657=AXIS2_PLACEMENT_3D('',#23367,#19184,#19185);
#15658=AXIS2_PLACEMENT_3D('',#23370,#19187,#19188);
#15659=AXIS2_PLACEMENT_3D('',#23371,#19189,#19190);
#15660=AXIS2_PLACEMENT_3D('',#23373,#19191,#19192);
#15661=AXIS2_PLACEMENT_3D('',#23376,#19194,#19195);
#15662=AXIS2_PLACEMENT_3D('',#23377,#19196,#19197);
#15663=AXIS2_PLACEMENT_3D('',#23378,#19198,#19199);
#15664=AXIS2_PLACEMENT_3D('',#23379,#19200,#19201);
#15665=AXIS2_PLACEMENT_3D('',#23380,#19202,#19203);
#15666=AXIS2_PLACEMENT_3D('',#23382,#19204,#19205);
#15667=AXIS2_PLACEMENT_3D('',#23385,#19207,#19208);
#15668=AXIS2_PLACEMENT_3D('',#23386,#19209,#19210);
#15669=AXIS2_PLACEMENT_3D('',#23388,#19211,#19212);
#15670=AXIS2_PLACEMENT_3D('',#23391,#19214,#19215);
#15671=AXIS2_PLACEMENT_3D('',#23392,#19216,#19217);
#15672=AXIS2_PLACEMENT_3D('',#23393,#19218,#19219);
#15673=AXIS2_PLACEMENT_3D('',#23394,#19220,#19221);
#15674=AXIS2_PLACEMENT_3D('',#23395,#19222,#19223);
#15675=AXIS2_PLACEMENT_3D('',#23397,#19224,#19225);
#15676=AXIS2_PLACEMENT_3D('',#23398,#19226,#19227);
#15677=AXIS2_PLACEMENT_3D('',#23400,#19228,#19229);
#15678=AXIS2_PLACEMENT_3D('',#23402,#19231,#19232);
#15679=AXIS2_PLACEMENT_3D('',#23404,#19233,#19234);
#15680=AXIS2_PLACEMENT_3D('',#23406,#19236,#19237);
#15681=AXIS2_PLACEMENT_3D('',#23408,#19238,#19239);
#15682=AXIS2_PLACEMENT_3D('',#23410,#19241,#19242);
#15683=AXIS2_PLACEMENT_3D('',#23412,#19243,#19244);
#15684=AXIS2_PLACEMENT_3D('',#23413,#19245,#19246);
#15685=AXIS2_PLACEMENT_3D('',#23415,#19247,#19248);
#15686=AXIS2_PLACEMENT_3D('',#23417,#19250,#19251);
#15687=AXIS2_PLACEMENT_3D('',#23419,#19252,#19253);
#15688=AXIS2_PLACEMENT_3D('',#23421,#19255,#19256);
#15689=AXIS2_PLACEMENT_3D('',#23423,#19257,#19258);
#15690=AXIS2_PLACEMENT_3D('',#23425,#19260,#19261);
#15691=AXIS2_PLACEMENT_3D('',#23426,#19262,#19263);
#15692=AXIS2_PLACEMENT_3D('',#23435,#19268,#19269);
#15693=AXIS2_PLACEMENT_3D('',#23441,#19273,#19274);
#15694=AXIS2_PLACEMENT_3D('',#23447,#19278,#19279);
#15695=AXIS2_PLACEMENT_3D('',#23453,#19283,#19284);
#15696=AXIS2_PLACEMENT_3D('',#23459,#19288,#19289);
#15697=AXIS2_PLACEMENT_3D('',#23462,#19292,#19293);
#15698=AXIS2_PLACEMENT_3D('',#23463,#19294,#19295);
#15699=AXIS2_PLACEMENT_3D('',#23464,#19296,#19297);
#15700=AXIS2_PLACEMENT_3D('',#23465,#19298,#19299);
#15701=AXIS2_PLACEMENT_3D('',#23466,#19300,#19301);
#15702=AXIS2_PLACEMENT_3D('',#23467,#19302,#19303);
#15703=AXIS2_PLACEMENT_3D('',#23468,#19304,#19305);
#15704=AXIS2_PLACEMENT_3D('',#23469,#19306,#19307);
#15705=AXIS2_PLACEMENT_3D('',#23470,#19308,#19309);
#15706=AXIS2_PLACEMENT_3D('',#23471,#19310,#19311);
#15707=AXIS2_PLACEMENT_3D('',#23472,#19312,#19313);
#15708=AXIS2_PLACEMENT_3D('',#23473,#19314,#19315);
#15709=AXIS2_PLACEMENT_3D('',#23474,#19316,#19317);
#15710=AXIS2_PLACEMENT_3D('',#23475,#19318,#19319);
#15711=AXIS2_PLACEMENT_3D('',#23476,#19320,#19321);
#15712=AXIS2_PLACEMENT_3D('',#23477,#19322,#19323);
#15713=AXIS2_PLACEMENT_3D('',#23478,#19324,#19325);
#15714=AXIS2_PLACEMENT_3D('',#23479,#19326,#19327);
#15715=AXIS2_PLACEMENT_3D('',#23480,#19328,#19329);
#15716=AXIS2_PLACEMENT_3D('',#23481,#19330,#19331);
#15717=AXIS2_PLACEMENT_3D('',#23482,#19332,#19333);
#15718=AXIS2_PLACEMENT_3D('',#23483,#19334,#19335);
#15719=AXIS2_PLACEMENT_3D('',#23484,#19336,#19337);
#15720=AXIS2_PLACEMENT_3D('',#23485,#19338,#19339);
#15721=AXIS2_PLACEMENT_3D('',#23486,#19340,#19341);
#15722=AXIS2_PLACEMENT_3D('',#23487,#19342,#19343);
#15723=AXIS2_PLACEMENT_3D('',#23488,#19344,#19345);
#15724=AXIS2_PLACEMENT_3D('',#23489,#19346,#19347);
#15725=AXIS2_PLACEMENT_3D('',#23490,#19348,#19349);
#15726=AXIS2_PLACEMENT_3D('',#23491,#19350,#19351);
#15727=AXIS2_PLACEMENT_3D('',#23492,#19352,#19353);
#15728=AXIS2_PLACEMENT_3D('',#23493,#19354,#19355);
#15729=AXIS2_PLACEMENT_3D('',#23494,#19356,#19357);
#15730=AXIS2_PLACEMENT_3D('',#23495,#19358,#19359);
#15731=AXIS2_PLACEMENT_3D('',#23496,#19360,#19361);
#15732=AXIS2_PLACEMENT_3D('',#23497,#19362,#19363);
#15733=AXIS2_PLACEMENT_3D('',#23498,#19364,#19365);
#15734=AXIS2_PLACEMENT_3D('',#23499,#19366,#19367);
#15735=AXIS2_PLACEMENT_3D('',#23500,#19368,#19369);
#15736=AXIS2_PLACEMENT_3D('',#23501,#19370,#19371);
#15737=AXIS2_PLACEMENT_3D('',#23502,#19372,#19373);
#15738=AXIS2_PLACEMENT_3D('',#23503,#19374,#19375);
#15739=AXIS2_PLACEMENT_3D('',#23504,#19376,#19377);
#15740=AXIS2_PLACEMENT_3D('',#23505,#19378,#19379);
#15741=AXIS2_PLACEMENT_3D('',#23506,#19380,#19381);
#15742=AXIS2_PLACEMENT_3D('',#23507,#19382,#19383);
#15743=AXIS2_PLACEMENT_3D('',#23508,#19384,#19385);
#15744=AXIS2_PLACEMENT_3D('',#23509,#19386,#19387);
#15745=AXIS2_PLACEMENT_3D('',#23510,#19388,#19389);
#15746=AXIS2_PLACEMENT_3D('',#23511,#19390,#19391);
#15747=AXIS2_PLACEMENT_3D('',#23512,#19392,#19393);
#15748=AXIS2_PLACEMENT_3D('',#23513,#19394,#19395);
#15749=AXIS2_PLACEMENT_3D('',#23514,#19396,#19397);
#15750=AXIS2_PLACEMENT_3D('',#23515,#19398,#19399);
#15751=AXIS2_PLACEMENT_3D('',#23516,#19400,#19401);
#15752=AXIS2_PLACEMENT_3D('',#23517,#19402,#19403);
#15753=AXIS2_PLACEMENT_3D('',#23518,#19404,#19405);
#15754=AXIS2_PLACEMENT_3D('',#23519,#19406,#19407);
#15755=AXIS2_PLACEMENT_3D('',#23520,#19408,#19409);
#15756=AXIS2_PLACEMENT_3D('',#23521,#19410,#19411);
#15757=AXIS2_PLACEMENT_3D('',#23522,#19412,#19413);
#15758=AXIS2_PLACEMENT_3D('',#23523,#19414,#19415);
#15759=AXIS2_PLACEMENT_3D('',#23524,#19416,#19417);
#15760=AXIS2_PLACEMENT_3D('',#23525,#19418,#19419);
#15761=AXIS2_PLACEMENT_3D('',#23526,#19420,#19421);
#15762=AXIS2_PLACEMENT_3D('',#23527,#19422,#19423);
#15763=AXIS2_PLACEMENT_3D('',#23528,#19424,#19425);
#15764=AXIS2_PLACEMENT_3D('',#23529,#19426,#19427);
#15765=AXIS2_PLACEMENT_3D('',#23530,#19428,#19429);
#15766=AXIS2_PLACEMENT_3D('',#23531,#19430,#19431);
#15767=AXIS2_PLACEMENT_3D('',#23532,#19432,#19433);
#15768=AXIS2_PLACEMENT_3D('',#23533,#19434,#19435);
#15769=AXIS2_PLACEMENT_3D('',#23534,#19436,#19437);
#15770=AXIS2_PLACEMENT_3D('',#23535,#19438,#19439);
#15771=AXIS2_PLACEMENT_3D('',#23536,#19440,#19441);
#15772=AXIS2_PLACEMENT_3D('',#23537,#19442,#19443);
#15773=AXIS2_PLACEMENT_3D('',#23538,#19444,#19445);
#15774=AXIS2_PLACEMENT_3D('',#23540,#19446,#19447);
#15775=AXIS2_PLACEMENT_3D('',#23543,#19449,#19450);
#15776=AXIS2_PLACEMENT_3D('',#23544,#19451,#19452);
#15777=AXIS2_PLACEMENT_3D('',#23546,#19453,#19454);
#15778=AXIS2_PLACEMENT_3D('',#23549,#19456,#19457);
#15779=AXIS2_PLACEMENT_3D('',#23550,#19458,#19459);
#15780=AXIS2_PLACEMENT_3D('',#23552,#19460,#19461);
#15781=AXIS2_PLACEMENT_3D('',#23555,#19463,#19464);
#15782=AXIS2_PLACEMENT_3D('',#23556,#19465,#19466);
#15783=AXIS2_PLACEMENT_3D('',#23558,#19467,#19468);
#15784=AXIS2_PLACEMENT_3D('',#23561,#19470,#19471);
#15785=AXIS2_PLACEMENT_3D('',#23562,#19472,#19473);
#15786=AXIS2_PLACEMENT_3D('',#23564,#19474,#19475);
#15787=AXIS2_PLACEMENT_3D('',#23567,#19477,#19478);
#15788=AXIS2_PLACEMENT_3D('',#23568,#19479,#19480);
#15789=AXIS2_PLACEMENT_3D('',#23573,#19482,#19483);
#15790=AXIS2_PLACEMENT_3D('',#23576,#19485,#19486);
#15791=AXIS2_PLACEMENT_3D('',#23577,#19487,#19488);
#15792=AXIS2_PLACEMENT_3D('',#23582,#19490,#19491);
#15793=AXIS2_PLACEMENT_3D('',#23585,#19493,#19494);
#15794=AXIS2_PLACEMENT_3D('',#23586,#19495,#19496);
#15795=AXIS2_PLACEMENT_3D('',#23592,#19500,#19501);
#15796=AXIS2_PLACEMENT_3D('',#23594,#19502,#19503);
#15797=AXIS2_PLACEMENT_3D('',#23599,#19506,#19507);
#15798=AXIS2_PLACEMENT_3D('',#23602,#19509,#19510);
#15799=AXIS2_PLACEMENT_3D('',#23604,#19511,#19512);
#15800=AXIS2_PLACEMENT_3D('',#23605,#19513,#19514);
#15801=AXIS2_PLACEMENT_3D('',#23609,#19517,#19518);
#15802=AXIS2_PLACEMENT_3D('',#23611,#19519,#19520);
#15803=AXIS2_PLACEMENT_3D('',#23613,#19522,#19523);
#15804=AXIS2_PLACEMENT_3D('',#23617,#19525,#19526);
#15805=AXIS2_PLACEMENT_3D('',#23619,#19528,#19529);
#15806=AXIS2_PLACEMENT_3D('',#23621,#19531,#19532);
#15807=AXIS2_PLACEMENT_3D('',#23623,#19533,#19534);
#15808=AXIS2_PLACEMENT_3D('',#23625,#19536,#19537);
#15809=AXIS2_PLACEMENT_3D('',#23626,#19538,#19539);
#15810=AXIS2_PLACEMENT_3D('',#23627,#19540,#19541);
#15811=AXIS2_PLACEMENT_3D('',#23629,#19543,#19544);
#15812=AXIS2_PLACEMENT_3D('',#23630,#19545,#19546);
#15813=AXIS2_PLACEMENT_3D('',#23631,#19547,#19548);
#15814=AXIS2_PLACEMENT_3D('',#23633,#19549,#19550);
#15815=AXIS2_PLACEMENT_3D('',#23636,#19552,#19553);
#15816=AXIS2_PLACEMENT_3D('',#23637,#19554,#19555);
#15817=AXIS2_PLACEMENT_3D('',#23639,#19556,#19557);
#15818=AXIS2_PLACEMENT_3D('',#23642,#19559,#19560);
#15819=AXIS2_PLACEMENT_3D('',#23643,#19561,#19562);
#15820=AXIS2_PLACEMENT_3D('',#23644,#19563,#19564);
#15821=AXIS2_PLACEMENT_3D('',#23645,#19565,#19566);
#15822=AXIS2_PLACEMENT_3D('',#23646,#19567,#19568);
#15823=AXIS2_PLACEMENT_3D('',#23648,#19569,#19570);
#15824=AXIS2_PLACEMENT_3D('',#23651,#19572,#19573);
#15825=AXIS2_PLACEMENT_3D('',#23652,#19574,#19575);
#15826=AXIS2_PLACEMENT_3D('',#23654,#19576,#19577);
#15827=AXIS2_PLACEMENT_3D('',#23657,#19579,#19580);
#15828=AXIS2_PLACEMENT_3D('',#23658,#19581,#19582);
#15829=AXIS2_PLACEMENT_3D('',#23659,#19583,#19584);
#15830=AXIS2_PLACEMENT_3D('',#23660,#19585,#19586);
#15831=AXIS2_PLACEMENT_3D('',#23661,#19587,#19588);
#15832=AXIS2_PLACEMENT_3D('',#23663,#19589,#19590);
#15833=AXIS2_PLACEMENT_3D('',#23666,#19592,#19593);
#15834=AXIS2_PLACEMENT_3D('',#23667,#19594,#19595);
#15835=AXIS2_PLACEMENT_3D('',#23669,#19596,#19597);
#15836=AXIS2_PLACEMENT_3D('',#23672,#19599,#19600);
#15837=AXIS2_PLACEMENT_3D('',#23673,#19601,#19602);
#15838=AXIS2_PLACEMENT_3D('',#23675,#19603,#19604);
#15839=AXIS2_PLACEMENT_3D('',#23678,#19606,#19607);
#15840=AXIS2_PLACEMENT_3D('',#23679,#19608,#19609);
#15841=AXIS2_PLACEMENT_3D('',#23681,#19610,#19611);
#15842=AXIS2_PLACEMENT_3D('',#23684,#19613,#19614);
#15843=AXIS2_PLACEMENT_3D('',#23685,#19615,#19616);
#15844=AXIS2_PLACEMENT_3D('',#23687,#19617,#19618);
#15845=AXIS2_PLACEMENT_3D('',#23690,#19620,#19621);
#15846=AXIS2_PLACEMENT_3D('',#23691,#19622,#19623);
#15847=AXIS2_PLACEMENT_3D('',#23693,#19624,#19625);
#15848=AXIS2_PLACEMENT_3D('',#23696,#19627,#19628);
#15849=AXIS2_PLACEMENT_3D('',#23697,#19629,#19630);
#15850=AXIS2_PLACEMENT_3D('',#23698,#19631,#19632);
#15851=AXIS2_PLACEMENT_3D('',#23699,#19633,#19634);
#15852=AXIS2_PLACEMENT_3D('',#23700,#19635,#19636);
#15853=AXIS2_PLACEMENT_3D('',#23702,#19637,#19638);
#15854=AXIS2_PLACEMENT_3D('',#23704,#19639,#19640);
#15855=AXIS2_PLACEMENT_3D('',#23705,#19641,#19642);
#15856=AXIS2_PLACEMENT_3D('',#23708,#19644,#19645);
#15857=AXIS2_PLACEMENT_3D('',#23709,#19646,#19647);
#15858=AXIS2_PLACEMENT_3D('',#23710,#19648,#19649);
#15859=AXIS2_PLACEMENT_3D('',#23712,#19650,#19651);
#15860=AXIS2_PLACEMENT_3D('',#23714,#19653,#19654);
#15861=AXIS2_PLACEMENT_3D('',#23715,#19655,#19656);
#15862=AXIS2_PLACEMENT_3D('',#23716,#19657,#19658);
#15863=AXIS2_PLACEMENT_3D('',#23718,#19659,#19660);
#15864=AXIS2_PLACEMENT_3D('',#23720,#19661,#19662);
#15865=AXIS2_PLACEMENT_3D('',#23721,#19663,#19664);
#15866=AXIS2_PLACEMENT_3D('',#23724,#19666,#19667);
#15867=AXIS2_PLACEMENT_3D('',#23725,#19668,#19669);
#15868=AXIS2_PLACEMENT_3D('',#23726,#19670,#19671);
#15869=AXIS2_PLACEMENT_3D('',#23728,#19672,#19673);
#15870=AXIS2_PLACEMENT_3D('',#23730,#19675,#19676);
#15871=AXIS2_PLACEMENT_3D('',#23731,#19677,#19678);
#15872=AXIS2_PLACEMENT_3D('',#23732,#19679,#19680);
#15873=AXIS2_PLACEMENT_3D('',#23734,#19681,#19682);
#15874=AXIS2_PLACEMENT_3D('',#23736,#19683,#19684);
#15875=AXIS2_PLACEMENT_3D('',#23737,#19685,#19686);
#15876=AXIS2_PLACEMENT_3D('',#23740,#19688,#19689);
#15877=AXIS2_PLACEMENT_3D('',#23741,#19690,#19691);
#15878=AXIS2_PLACEMENT_3D('',#23742,#19692,#19693);
#15879=AXIS2_PLACEMENT_3D('',#23744,#19694,#19695);
#15880=AXIS2_PLACEMENT_3D('',#23746,#19697,#19698);
#15881=AXIS2_PLACEMENT_3D('',#23747,#19699,#19700);
#15882=AXIS2_PLACEMENT_3D('',#23748,#19701,#19702);
#15883=AXIS2_PLACEMENT_3D('',#23750,#19703,#19704);
#15884=AXIS2_PLACEMENT_3D('',#23752,#19705,#19706);
#15885=AXIS2_PLACEMENT_3D('',#23753,#19707,#19708);
#15886=AXIS2_PLACEMENT_3D('',#23756,#19710,#19711);
#15887=AXIS2_PLACEMENT_3D('',#23757,#19712,#19713);
#15888=AXIS2_PLACEMENT_3D('',#23758,#19714,#19715);
#15889=AXIS2_PLACEMENT_3D('',#23760,#19716,#19717);
#15890=AXIS2_PLACEMENT_3D('',#23762,#19719,#19720);
#15891=AXIS2_PLACEMENT_3D('',#23763,#19721,#19722);
#15892=AXIS2_PLACEMENT_3D('',#23764,#19723,#19724);
#15893=AXIS2_PLACEMENT_3D('',#23766,#19725,#19726);
#15894=AXIS2_PLACEMENT_3D('',#23769,#19728,#19729);
#15895=AXIS2_PLACEMENT_3D('',#23770,#19730,#19731);
#15896=AXIS2_PLACEMENT_3D('',#23772,#19732,#19733);
#15897=AXIS2_PLACEMENT_3D('',#23775,#19735,#19736);
#15898=AXIS2_PLACEMENT_3D('',#23776,#19737,#19738);
#15899=AXIS2_PLACEMENT_3D('',#23778,#19739,#19740);
#15900=AXIS2_PLACEMENT_3D('',#23781,#19742,#19743);
#15901=AXIS2_PLACEMENT_3D('',#23782,#19744,#19745);
#15902=AXIS2_PLACEMENT_3D('',#23784,#19746,#19747);
#15903=AXIS2_PLACEMENT_3D('',#23787,#19749,#19750);
#15904=AXIS2_PLACEMENT_3D('',#23788,#19751,#19752);
#15905=AXIS2_PLACEMENT_3D('',#23790,#19753,#19754);
#15906=AXIS2_PLACEMENT_3D('',#23793,#19756,#19757);
#15907=AXIS2_PLACEMENT_3D('',#23794,#19758,#19759);
#15908=AXIS2_PLACEMENT_3D('',#23796,#19760,#19761);
#15909=AXIS2_PLACEMENT_3D('',#23799,#19763,#19764);
#15910=AXIS2_PLACEMENT_3D('',#23800,#19765,#19766);
#15911=AXIS2_PLACEMENT_3D('',#23801,#19767,#19768);
#15912=AXIS2_PLACEMENT_3D('',#23802,#19769,#19770);
#15913=AXIS2_PLACEMENT_3D('',#23803,#19771,#19772);
#15914=AXIS2_PLACEMENT_3D('',#23805,#19773,#19774);
#15915=AXIS2_PLACEMENT_3D('',#23807,#19775,#19776);
#15916=AXIS2_PLACEMENT_3D('',#23808,#19777,#19778);
#15917=AXIS2_PLACEMENT_3D('',#23810,#19779,#19780);
#15918=AXIS2_PLACEMENT_3D('',#23812,#19782,#19783);
#15919=AXIS2_PLACEMENT_3D('',#23813,#19784,#19785);
#15920=AXIS2_PLACEMENT_3D('',#23816,#19787,#19788);
#15921=AXIS2_PLACEMENT_3D('',#23817,#19789,#19790);
#15922=AXIS2_PLACEMENT_3D('',#23818,#19791,#19792);
#15923=AXIS2_PLACEMENT_3D('',#23819,#19793,#19794);
#15924=AXIS2_PLACEMENT_3D('',#23821,#19795,#19796);
#15925=AXIS2_PLACEMENT_3D('',#23823,#19797,#19798);
#15926=AXIS2_PLACEMENT_3D('',#23824,#19799,#19800);
#15927=AXIS2_PLACEMENT_3D('',#23826,#19801,#19802);
#15928=AXIS2_PLACEMENT_3D('',#23828,#19804,#19805);
#15929=AXIS2_PLACEMENT_3D('',#23829,#19806,#19807);
#15930=AXIS2_PLACEMENT_3D('',#23832,#19809,#19810);
#15931=AXIS2_PLACEMENT_3D('',#23833,#19811,#19812);
#15932=AXIS2_PLACEMENT_3D('',#23834,#19813,#19814);
#15933=AXIS2_PLACEMENT_3D('',#23835,#19815,#19816);
#15934=AXIS2_PLACEMENT_3D('',#23837,#19817,#19818);
#15935=AXIS2_PLACEMENT_3D('',#23839,#19819,#19820);
#15936=AXIS2_PLACEMENT_3D('',#23840,#19821,#19822);
#15937=AXIS2_PLACEMENT_3D('',#23842,#19823,#19824);
#15938=AXIS2_PLACEMENT_3D('',#23844,#19826,#19827);
#15939=AXIS2_PLACEMENT_3D('',#23845,#19828,#19829);
#15940=AXIS2_PLACEMENT_3D('',#23848,#19831,#19832);
#15941=AXIS2_PLACEMENT_3D('',#23849,#19833,#19834);
#15942=AXIS2_PLACEMENT_3D('',#23850,#19835,#19836);
#15943=AXIS2_PLACEMENT_3D('',#23851,#19837,#19838);
#15944=AXIS2_PLACEMENT_3D('',#23853,#19839,#19840);
#15945=AXIS2_PLACEMENT_3D('',#23855,#19841,#19842);
#15946=AXIS2_PLACEMENT_3D('',#23856,#19843,#19844);
#15947=AXIS2_PLACEMENT_3D('',#23858,#19845,#19846);
#15948=AXIS2_PLACEMENT_3D('',#23860,#19848,#19849);
#15949=AXIS2_PLACEMENT_3D('',#23861,#19850,#19851);
#15950=AXIS2_PLACEMENT_3D('',#23864,#19853,#19854);
#15951=AXIS2_PLACEMENT_3D('',#23865,#19855,#19856);
#15952=AXIS2_PLACEMENT_3D('',#23866,#19857,#19858);
#15953=AXIS2_PLACEMENT_3D('',#23867,#19859,#19860);
#15954=AXIS2_PLACEMENT_3D('',#23869,#19861,#19862);
#15955=AXIS2_PLACEMENT_3D('',#23872,#19864,#19865);
#15956=AXIS2_PLACEMENT_3D('',#23873,#19866,#19867);
#15957=AXIS2_PLACEMENT_3D('',#23875,#19868,#19869);
#15958=AXIS2_PLACEMENT_3D('',#23878,#19871,#19872);
#15959=AXIS2_PLACEMENT_3D('',#23879,#19873,#19874);
#15960=AXIS2_PLACEMENT_3D('',#23881,#19875,#19876);
#15961=AXIS2_PLACEMENT_3D('',#23884,#19878,#19879);
#15962=AXIS2_PLACEMENT_3D('',#23885,#19880,#19881);
#15963=AXIS2_PLACEMENT_3D('',#23887,#19882,#19883);
#15964=AXIS2_PLACEMENT_3D('',#23890,#19885,#19886);
#15965=AXIS2_PLACEMENT_3D('',#23891,#19887,#19888);
#15966=AXIS2_PLACEMENT_3D('',#23893,#19889,#19890);
#15967=AXIS2_PLACEMENT_3D('',#23896,#19892,#19893);
#15968=AXIS2_PLACEMENT_3D('',#23897,#19894,#19895);
#15969=AXIS2_PLACEMENT_3D('',#23902,#19897,#19898);
#15970=AXIS2_PLACEMENT_3D('',#23905,#19900,#19901);
#15971=AXIS2_PLACEMENT_3D('',#23906,#19902,#19903);
#15972=AXIS2_PLACEMENT_3D('',#23911,#19905,#19906);
#15973=AXIS2_PLACEMENT_3D('',#23914,#19908,#19909);
#15974=AXIS2_PLACEMENT_3D('',#23915,#19910,#19911);
#15975=AXIS2_PLACEMENT_3D('',#23921,#19915,#19916);
#15976=AXIS2_PLACEMENT_3D('',#23923,#19917,#19918);
#15977=AXIS2_PLACEMENT_3D('',#23928,#19921,#19922);
#15978=AXIS2_PLACEMENT_3D('',#23931,#19924,#19925);
#15979=AXIS2_PLACEMENT_3D('',#23933,#19926,#19927);
#15980=AXIS2_PLACEMENT_3D('',#23934,#19928,#19929);
#15981=AXIS2_PLACEMENT_3D('',#23938,#19932,#19933);
#15982=AXIS2_PLACEMENT_3D('',#23940,#19934,#19935);
#15983=AXIS2_PLACEMENT_3D('',#23942,#19937,#19938);
#15984=AXIS2_PLACEMENT_3D('',#23946,#19940,#19941);
#15985=AXIS2_PLACEMENT_3D('',#23948,#19943,#19944);
#15986=AXIS2_PLACEMENT_3D('',#23950,#19946,#19947);
#15987=AXIS2_PLACEMENT_3D('',#23952,#19948,#19949);
#15988=AXIS2_PLACEMENT_3D('',#23954,#19951,#19952);
#15989=AXIS2_PLACEMENT_3D('',#23955,#19953,#19954);
#15990=AXIS2_PLACEMENT_3D('',#23956,#19955,#19956);
#15991=AXIS2_PLACEMENT_3D('',#23958,#19958,#19959);
#15992=AXIS2_PLACEMENT_3D('',#23959,#19960,#19961);
#15993=AXIS2_PLACEMENT_3D('',#23960,#19962,#19963);
#15994=AXIS2_PLACEMENT_3D('',#23962,#19964,#19965);
#15995=AXIS2_PLACEMENT_3D('',#23965,#19967,#19968);
#15996=AXIS2_PLACEMENT_3D('',#23966,#19969,#19970);
#15997=AXIS2_PLACEMENT_3D('',#23968,#19971,#19972);
#15998=AXIS2_PLACEMENT_3D('',#23971,#19974,#19975);
#15999=AXIS2_PLACEMENT_3D('',#23972,#19976,#19977);
#16000=AXIS2_PLACEMENT_3D('',#23973,#19978,#19979);
#16001=AXIS2_PLACEMENT_3D('',#23974,#19980,#19981);
#16002=AXIS2_PLACEMENT_3D('',#23975,#19982,#19983);
#16003=AXIS2_PLACEMENT_3D('',#23977,#19984,#19985);
#16004=AXIS2_PLACEMENT_3D('',#23980,#19987,#19988);
#16005=AXIS2_PLACEMENT_3D('',#23981,#19989,#19990);
#16006=AXIS2_PLACEMENT_3D('',#23983,#19991,#19992);
#16007=AXIS2_PLACEMENT_3D('',#23986,#19994,#19995);
#16008=AXIS2_PLACEMENT_3D('',#23987,#19996,#19997);
#16009=AXIS2_PLACEMENT_3D('',#23988,#19998,#19999);
#16010=AXIS2_PLACEMENT_3D('',#23989,#20000,#20001);
#16011=AXIS2_PLACEMENT_3D('',#23990,#20002,#20003);
#16012=AXIS2_PLACEMENT_3D('',#23992,#20004,#20005);
#16013=AXIS2_PLACEMENT_3D('',#23995,#20007,#20008);
#16014=AXIS2_PLACEMENT_3D('',#23996,#20009,#20010);
#16015=AXIS2_PLACEMENT_3D('',#23998,#20011,#20012);
#16016=AXIS2_PLACEMENT_3D('',#24001,#20014,#20015);
#16017=AXIS2_PLACEMENT_3D('',#24002,#20016,#20017);
#16018=AXIS2_PLACEMENT_3D('',#24004,#20018,#20019);
#16019=AXIS2_PLACEMENT_3D('',#24007,#20021,#20022);
#16020=AXIS2_PLACEMENT_3D('',#24008,#20023,#20024);
#16021=AXIS2_PLACEMENT_3D('',#24010,#20025,#20026);
#16022=AXIS2_PLACEMENT_3D('',#24013,#20028,#20029);
#16023=AXIS2_PLACEMENT_3D('',#24014,#20030,#20031);
#16024=AXIS2_PLACEMENT_3D('',#24016,#20032,#20033);
#16025=AXIS2_PLACEMENT_3D('',#24019,#20035,#20036);
#16026=AXIS2_PLACEMENT_3D('',#24020,#20037,#20038);
#16027=AXIS2_PLACEMENT_3D('',#24022,#20039,#20040);
#16028=AXIS2_PLACEMENT_3D('',#24025,#20042,#20043);
#16029=AXIS2_PLACEMENT_3D('',#24026,#20044,#20045);
#16030=AXIS2_PLACEMENT_3D('',#24027,#20046,#20047);
#16031=AXIS2_PLACEMENT_3D('',#24028,#20048,#20049);
#16032=AXIS2_PLACEMENT_3D('',#24029,#20050,#20051);
#16033=AXIS2_PLACEMENT_3D('',#24031,#20052,#20053);
#16034=AXIS2_PLACEMENT_3D('',#24033,#20054,#20055);
#16035=AXIS2_PLACEMENT_3D('',#24034,#20056,#20057);
#16036=AXIS2_PLACEMENT_3D('',#24037,#20059,#20060);
#16037=AXIS2_PLACEMENT_3D('',#24038,#20061,#20062);
#16038=AXIS2_PLACEMENT_3D('',#24039,#20063,#20064);
#16039=AXIS2_PLACEMENT_3D('',#24041,#20065,#20066);
#16040=AXIS2_PLACEMENT_3D('',#24043,#20068,#20069);
#16041=AXIS2_PLACEMENT_3D('',#24044,#20070,#20071);
#16042=AXIS2_PLACEMENT_3D('',#24045,#20072,#20073);
#16043=AXIS2_PLACEMENT_3D('',#24047,#20074,#20075);
#16044=AXIS2_PLACEMENT_3D('',#24049,#20076,#20077);
#16045=AXIS2_PLACEMENT_3D('',#24050,#20078,#20079);
#16046=AXIS2_PLACEMENT_3D('',#24053,#20081,#20082);
#16047=AXIS2_PLACEMENT_3D('',#24054,#20083,#20084);
#16048=AXIS2_PLACEMENT_3D('',#24055,#20085,#20086);
#16049=AXIS2_PLACEMENT_3D('',#24057,#20087,#20088);
#16050=AXIS2_PLACEMENT_3D('',#24059,#20090,#20091);
#16051=AXIS2_PLACEMENT_3D('',#24060,#20092,#20093);
#16052=AXIS2_PLACEMENT_3D('',#24061,#20094,#20095);
#16053=AXIS2_PLACEMENT_3D('',#24063,#20096,#20097);
#16054=AXIS2_PLACEMENT_3D('',#24065,#20098,#20099);
#16055=AXIS2_PLACEMENT_3D('',#24066,#20100,#20101);
#16056=AXIS2_PLACEMENT_3D('',#24069,#20103,#20104);
#16057=AXIS2_PLACEMENT_3D('',#24070,#20105,#20106);
#16058=AXIS2_PLACEMENT_3D('',#24071,#20107,#20108);
#16059=AXIS2_PLACEMENT_3D('',#24073,#20109,#20110);
#16060=AXIS2_PLACEMENT_3D('',#24075,#20112,#20113);
#16061=AXIS2_PLACEMENT_3D('',#24076,#20114,#20115);
#16062=AXIS2_PLACEMENT_3D('',#24077,#20116,#20117);
#16063=AXIS2_PLACEMENT_3D('',#24079,#20118,#20119);
#16064=AXIS2_PLACEMENT_3D('',#24081,#20120,#20121);
#16065=AXIS2_PLACEMENT_3D('',#24082,#20122,#20123);
#16066=AXIS2_PLACEMENT_3D('',#24085,#20125,#20126);
#16067=AXIS2_PLACEMENT_3D('',#24086,#20127,#20128);
#16068=AXIS2_PLACEMENT_3D('',#24087,#20129,#20130);
#16069=AXIS2_PLACEMENT_3D('',#24089,#20131,#20132);
#16070=AXIS2_PLACEMENT_3D('',#24091,#20134,#20135);
#16071=AXIS2_PLACEMENT_3D('',#24092,#20136,#20137);
#16072=AXIS2_PLACEMENT_3D('',#24093,#20138,#20139);
#16073=AXIS2_PLACEMENT_3D('',#24095,#20140,#20141);
#16074=AXIS2_PLACEMENT_3D('',#24098,#20143,#20144);
#16075=AXIS2_PLACEMENT_3D('',#24099,#20145,#20146);
#16076=AXIS2_PLACEMENT_3D('',#24101,#20147,#20148);
#16077=AXIS2_PLACEMENT_3D('',#24104,#20150,#20151);
#16078=AXIS2_PLACEMENT_3D('',#24105,#20152,#20153);
#16079=AXIS2_PLACEMENT_3D('',#24107,#20154,#20155);
#16080=AXIS2_PLACEMENT_3D('',#24110,#20157,#20158);
#16081=AXIS2_PLACEMENT_3D('',#24111,#20159,#20160);
#16082=AXIS2_PLACEMENT_3D('',#24113,#20161,#20162);
#16083=AXIS2_PLACEMENT_3D('',#24116,#20164,#20165);
#16084=AXIS2_PLACEMENT_3D('',#24117,#20166,#20167);
#16085=AXIS2_PLACEMENT_3D('',#24119,#20168,#20169);
#16086=AXIS2_PLACEMENT_3D('',#24122,#20171,#20172);
#16087=AXIS2_PLACEMENT_3D('',#24123,#20173,#20174);
#16088=AXIS2_PLACEMENT_3D('',#24125,#20175,#20176);
#16089=AXIS2_PLACEMENT_3D('',#24128,#20178,#20179);
#16090=AXIS2_PLACEMENT_3D('',#24129,#20180,#20181);
#16091=AXIS2_PLACEMENT_3D('',#24130,#20182,#20183);
#16092=AXIS2_PLACEMENT_3D('',#24131,#20184,#20185);
#16093=AXIS2_PLACEMENT_3D('',#24132,#20186,#20187);
#16094=AXIS2_PLACEMENT_3D('',#24134,#20188,#20189);
#16095=AXIS2_PLACEMENT_3D('',#24136,#20190,#20191);
#16096=AXIS2_PLACEMENT_3D('',#24137,#20192,#20193);
#16097=AXIS2_PLACEMENT_3D('',#24139,#20194,#20195);
#16098=AXIS2_PLACEMENT_3D('',#24141,#20197,#20198);
#16099=AXIS2_PLACEMENT_3D('',#24142,#20199,#20200);
#16100=AXIS2_PLACEMENT_3D('',#24145,#20202,#20203);
#16101=AXIS2_PLACEMENT_3D('',#24146,#20204,#20205);
#16102=AXIS2_PLACEMENT_3D('',#24147,#20206,#20207);
#16103=AXIS2_PLACEMENT_3D('',#24148,#20208,#20209);
#16104=AXIS2_PLACEMENT_3D('',#24150,#20210,#20211);
#16105=AXIS2_PLACEMENT_3D('',#24152,#20212,#20213);
#16106=AXIS2_PLACEMENT_3D('',#24153,#20214,#20215);
#16107=AXIS2_PLACEMENT_3D('',#24155,#20216,#20217);
#16108=AXIS2_PLACEMENT_3D('',#24157,#20219,#20220);
#16109=AXIS2_PLACEMENT_3D('',#24158,#20221,#20222);
#16110=AXIS2_PLACEMENT_3D('',#24161,#20224,#20225);
#16111=AXIS2_PLACEMENT_3D('',#24162,#20226,#20227);
#16112=AXIS2_PLACEMENT_3D('',#24163,#20228,#20229);
#16113=AXIS2_PLACEMENT_3D('',#24164,#20230,#20231);
#16114=AXIS2_PLACEMENT_3D('',#24166,#20232,#20233);
#16115=AXIS2_PLACEMENT_3D('',#24168,#20234,#20235);
#16116=AXIS2_PLACEMENT_3D('',#24169,#20236,#20237);
#16117=AXIS2_PLACEMENT_3D('',#24171,#20238,#20239);
#16118=AXIS2_PLACEMENT_3D('',#24173,#20241,#20242);
#16119=AXIS2_PLACEMENT_3D('',#24174,#20243,#20244);
#16120=AXIS2_PLACEMENT_3D('',#24177,#20246,#20247);
#16121=AXIS2_PLACEMENT_3D('',#24178,#20248,#20249);
#16122=AXIS2_PLACEMENT_3D('',#24179,#20250,#20251);
#16123=AXIS2_PLACEMENT_3D('',#24180,#20252,#20253);
#16124=AXIS2_PLACEMENT_3D('',#24182,#20254,#20255);
#16125=AXIS2_PLACEMENT_3D('',#24184,#20256,#20257);
#16126=AXIS2_PLACEMENT_3D('',#24185,#20258,#20259);
#16127=AXIS2_PLACEMENT_3D('',#24187,#20260,#20261);
#16128=AXIS2_PLACEMENT_3D('',#24189,#20263,#20264);
#16129=AXIS2_PLACEMENT_3D('',#24190,#20265,#20266);
#16130=AXIS2_PLACEMENT_3D('',#24193,#20268,#20269);
#16131=AXIS2_PLACEMENT_3D('',#24194,#20270,#20271);
#16132=AXIS2_PLACEMENT_3D('',#24195,#20272,#20273);
#16133=AXIS2_PLACEMENT_3D('',#24196,#20274,#20275);
#16134=AXIS2_PLACEMENT_3D('',#24197,#20276,#20277);
#16135=AXIS2_PLACEMENT_3D('',#24200,#20278,#20279);
#16136=AXIS2_PLACEMENT_3D('',#24201,#20280,#20281);
#16137=AXIS2_PLACEMENT_3D('',#24203,#20282,#20283);
#16138=AXIS2_PLACEMENT_3D('',#24205,#20284,#20285);
#16139=AXIS2_PLACEMENT_3D('',#24206,#20286,#20287);
#16140=AXIS2_PLACEMENT_3D('',#24207,#20288,#20289);
#16141=AXIS2_PLACEMENT_3D('',#24210,#20291,#20292);
#16142=AXIS2_PLACEMENT_3D('',#24211,#20293,#20294);
#16143=AXIS2_PLACEMENT_3D('',#24213,#20295,#20296);
#16144=AXIS2_PLACEMENT_3D('',#24216,#20298,#20299);
#16145=AXIS2_PLACEMENT_3D('',#24217,#20300,#20301);
#16146=AXIS2_PLACEMENT_3D('',#24220,#20303,#20304);
#16147=AXIS2_PLACEMENT_3D('',#24221,#20305,#20306);
#16148=AXIS2_PLACEMENT_3D('',#24222,#20307,#20308);
#16149=AXIS2_PLACEMENT_3D('',#24224,#20309,#20310);
#16150=AXIS2_PLACEMENT_3D('',#24226,#20312,#20313);
#16151=AXIS2_PLACEMENT_3D('',#24228,#20314,#20315);
#16152=AXIS2_PLACEMENT_3D('',#24229,#20316,#20317);
#16153=AXIS2_PLACEMENT_3D('',#24231,#20319,#20320);
#16154=AXIS2_PLACEMENT_3D('',#24232,#20321,#20322);
#16155=AXIS2_PLACEMENT_3D('',#24235,#20323,#20324);
#16156=AXIS2_PLACEMENT_3D('',#24236,#20325,#20326);
#16157=AXIS2_PLACEMENT_3D('',#24238,#20327,#20328);
#16158=AXIS2_PLACEMENT_3D('',#24240,#20329,#20330);
#16159=AXIS2_PLACEMENT_3D('',#24241,#20331,#20332);
#16160=AXIS2_PLACEMENT_3D('',#24242,#20333,#20334);
#16161=AXIS2_PLACEMENT_3D('',#24244,#20335,#20336);
#16162=AXIS2_PLACEMENT_3D('',#24246,#20338,#20339);
#16163=AXIS2_PLACEMENT_3D('',#24248,#20340,#20341);
#16164=AXIS2_PLACEMENT_3D('',#24250,#20342,#20343);
#16165=AXIS2_PLACEMENT_3D('',#24251,#20344,#20345);
#16166=AXIS2_PLACEMENT_3D('',#24253,#20346,#20347);
#16167=AXIS2_PLACEMENT_3D('',#24255,#20349,#20350);
#16168=AXIS2_PLACEMENT_3D('',#24257,#20351,#20352);
#16169=AXIS2_PLACEMENT_3D('',#24259,#20354,#20355);
#16170=AXIS2_PLACEMENT_3D('',#24261,#20356,#20357);
#16171=AXIS2_PLACEMENT_3D('',#24263,#20359,#20360);
#16172=AXIS2_PLACEMENT_3D('',#24264,#20361,#20362);
#16173=AXIS2_PLACEMENT_3D('',#24266,#20364,#20365);
#16174=AXIS2_PLACEMENT_3D('',#24267,#20366,#20367);
#16175=AXIS2_PLACEMENT_3D('',#24270,#20368,#20369);
#16176=AXIS2_PLACEMENT_3D('',#24271,#20370,#20371);
#16177=AXIS2_PLACEMENT_3D('',#24274,#20372,#20373);
#16178=AXIS2_PLACEMENT_3D('',#24275,#20374,#20375);
#16179=AXIS2_PLACEMENT_3D('',#24278,#20376,#20377);
#16180=AXIS2_PLACEMENT_3D('',#24279,#20378,#20379);
#16181=AXIS2_PLACEMENT_3D('',#24282,#20380,#20381);
#16182=AXIS2_PLACEMENT_3D('',#24283,#20382,#20383);
#16183=AXIS2_PLACEMENT_3D('',#24286,#20384,#20385);
#16184=AXIS2_PLACEMENT_3D('',#24287,#20386,#20387);
#16185=AXIS2_PLACEMENT_3D('',#24290,#20388,#20389);
#16186=AXIS2_PLACEMENT_3D('',#24291,#20390,#20391);
#16187=AXIS2_PLACEMENT_3D('',#24294,#20392,#20393);
#16188=AXIS2_PLACEMENT_3D('',#24295,#20394,#20395);
#16189=AXIS2_PLACEMENT_3D('',#24296,#20396,#20397);
#16190=AXIS2_PLACEMENT_3D('',#24306,#20398,#20399);
#16191=AXIS2_PLACEMENT_3D('',#24314,#20400,#20401);
#16192=AXIS2_PLACEMENT_3D('',#24315,#20402,#20403);
#16193=AXIS2_PLACEMENT_3D('',#24317,#20404,#20405);
#16194=AXIS2_PLACEMENT_3D('',#24319,#20406,#20407);
#16195=AXIS2_PLACEMENT_3D('',#24320,#20408,#20409);
#16196=AXIS2_PLACEMENT_3D('',#24321,#20410,#20411);
#16197=AXIS2_PLACEMENT_3D('',#24323,#20412,#20413);
#16198=AXIS2_PLACEMENT_3D('',#24330,#20414,#20415);
#16199=AXIS2_PLACEMENT_3D('',#24332,#20416,#20417);
#16200=AXIS2_PLACEMENT_3D('',#24333,#20418,#20419);
#16201=AXIS2_PLACEMENT_3D('',#24334,#20420,#20421);
#16202=AXIS2_PLACEMENT_3D('',#24341,#20422,#20423);
#16203=AXIS2_PLACEMENT_3D('',#24342,#20424,#20425);
#16204=AXIS2_PLACEMENT_3D('',#24345,#20426,#20427);
#16205=AXIS2_PLACEMENT_3D('',#24354,#20428,#20429);
#16206=AXIS2_PLACEMENT_3D('',#24361,#20430,#20431);
#16207=AXIS2_PLACEMENT_3D('',#24363,#20432,#20433);
#16208=AXIS2_PLACEMENT_3D('',#24365,#20434,#20435);
#16209=AXIS2_PLACEMENT_3D('',#24366,#20436,#20437);
#16210=AXIS2_PLACEMENT_3D('',#24367,#20438,#20439);
#16211=AXIS2_PLACEMENT_3D('',#24375,#20440,#20441);
#16212=AXIS2_PLACEMENT_3D('',#24376,#20442,#20443);
#16213=AXIS2_PLACEMENT_3D('',#24378,#20444,#20445);
#16214=AXIS2_PLACEMENT_3D('',#24385,#20446,#20447);
#16215=AXIS2_PLACEMENT_3D('',#24386,#20448,#20449);
#16216=AXIS2_PLACEMENT_3D('',#24387,#20450,#20451);
#16217=AXIS2_PLACEMENT_3D('',#24388,#20452,#20453);
#16218=AXIS2_PLACEMENT_3D('',#24398,#20454,#20455);
#16219=AXIS2_PLACEMENT_3D('',#24406,#20456,#20457);
#16220=AXIS2_PLACEMENT_3D('',#24407,#20458,#20459);
#16221=AXIS2_PLACEMENT_3D('',#24409,#20460,#20461);
#16222=AXIS2_PLACEMENT_3D('',#24417,#20462,#20463);
#16223=AXIS2_PLACEMENT_3D('',#24418,#20464,#20465);
#16224=AXIS2_PLACEMENT_3D('',#24420,#20466,#20467);
#16225=AXIS2_PLACEMENT_3D('',#24421,#20468,#20469);
#16226=AXIS2_PLACEMENT_3D('',#24422,#20470,#20471);
#16227=AXIS2_PLACEMENT_3D('',#24424,#20472,#20473);
#16228=AXIS2_PLACEMENT_3D('',#24425,#20474,#20475);
#16229=AXIS2_PLACEMENT_3D('',#24426,#20476,#20477);
#16230=AXIS2_PLACEMENT_3D('',#24433,#20478,#20479);
#16231=AXIS2_PLACEMENT_3D('',#24434,#20480,#20481);
#16232=AXIS2_PLACEMENT_3D('',#24437,#20482,#20483);
#16233=AXIS2_PLACEMENT_3D('',#24446,#20484,#20485);
#16234=AXIS2_PLACEMENT_3D('',#24453,#20486,#20487);
#16235=AXIS2_PLACEMENT_3D('',#24455,#20488,#20489);
#16236=AXIS2_PLACEMENT_3D('',#24463,#20490,#20491);
#16237=AXIS2_PLACEMENT_3D('',#24464,#20492,#20493);
#16238=AXIS2_PLACEMENT_3D('',#24466,#20494,#20495);
#16239=AXIS2_PLACEMENT_3D('',#24467,#20496,#20497);
#16240=AXIS2_PLACEMENT_3D('',#24468,#20498,#20499);
#16241=AXIS2_PLACEMENT_3D('',#24470,#20500,#20501);
#16242=AXIS2_PLACEMENT_3D('',#24477,#20502,#20503);
#16243=AXIS2_PLACEMENT_3D('',#24478,#20504,#20505);
#16244=AXIS2_PLACEMENT_3D('',#24479,#20506,#20507);
#16245=AXIS2_PLACEMENT_3D('',#24480,#20508,#20509);
#16246=AXIS2_PLACEMENT_3D('',#24490,#20510,#20511);
#16247=AXIS2_PLACEMENT_3D('',#24498,#20512,#20513);
#16248=AXIS2_PLACEMENT_3D('',#24499,#20514,#20515);
#16249=AXIS2_PLACEMENT_3D('',#24508,#20516,#20517);
#16250=AXIS2_PLACEMENT_3D('',#24509,#20518,#20519);
#16251=AXIS2_PLACEMENT_3D('',#24510,#20520,#20521);
#16252=AXIS2_PLACEMENT_3D('',#24512,#20522,#20523);
#16253=AXIS2_PLACEMENT_3D('',#24513,#20524,#20525);
#16254=AXIS2_PLACEMENT_3D('',#24514,#20526,#20527);
#16255=AXIS2_PLACEMENT_3D('',#24516,#20528,#20529);
#16256=AXIS2_PLACEMENT_3D('',#24517,#20530,#20531);
#16257=AXIS2_PLACEMENT_3D('',#24518,#20532,#20533);
#16258=AXIS2_PLACEMENT_3D('',#24525,#20534,#20535);
#16259=AXIS2_PLACEMENT_3D('',#24526,#20536,#20537);
#16260=AXIS2_PLACEMENT_3D('',#24536,#20538,#20539);
#16261=AXIS2_PLACEMENT_3D('',#24544,#20540,#20541);
#16262=AXIS2_PLACEMENT_3D('',#24545,#20542,#20543);
#16263=AXIS2_PLACEMENT_3D('',#24554,#20544,#20545);
#16264=AXIS2_PLACEMENT_3D('',#24555,#20546,#20547);
#16265=AXIS2_PLACEMENT_3D('',#24556,#20548,#20549);
#16266=AXIS2_PLACEMENT_3D('',#24558,#20550,#20551);
#16267=AXIS2_PLACEMENT_3D('',#24559,#20552,#20553);
#16268=AXIS2_PLACEMENT_3D('',#24560,#20554,#20555);
#16269=AXIS2_PLACEMENT_3D('',#24568,#20556,#20557);
#16270=AXIS2_PLACEMENT_3D('',#24569,#20558,#20559);
#16271=AXIS2_PLACEMENT_3D('',#24570,#20560,#20561);
#16272=AXIS2_PLACEMENT_3D('',#24571,#20562,#20563);
#16273=AXIS2_PLACEMENT_3D('',#24572,#20564,#20565);
#16274=AXIS2_PLACEMENT_3D('',#24582,#20566,#20567);
#16275=AXIS2_PLACEMENT_3D('',#24590,#20568,#20569);
#16276=AXIS2_PLACEMENT_3D('',#24591,#20570,#20571);
#16277=AXIS2_PLACEMENT_3D('',#24593,#20572,#20573);
#16278=AXIS2_PLACEMENT_3D('',#24595,#20574,#20575);
#16279=AXIS2_PLACEMENT_3D('',#24596,#20576,#20577);
#16280=AXIS2_PLACEMENT_3D('',#24597,#20578,#20579);
#16281=AXIS2_PLACEMENT_3D('',#24599,#20580,#20581);
#16282=AXIS2_PLACEMENT_3D('',#24606,#20582,#20583);
#16283=AXIS2_PLACEMENT_3D('',#24608,#20584,#20585);
#16284=AXIS2_PLACEMENT_3D('',#24609,#20586,#20587);
#16285=AXIS2_PLACEMENT_3D('',#24610,#20588,#20589);
#16286=AXIS2_PLACEMENT_3D('',#24617,#20590,#20591);
#16287=AXIS2_PLACEMENT_3D('',#24618,#20592,#20593);
#16288=AXIS2_PLACEMENT_3D('',#24619,#20594,#20595);
#16289=AXIS2_PLACEMENT_3D('',#24621,#20596,#20597);
#16290=AXIS2_PLACEMENT_3D('',#24623,#20598,#20599);
#16291=AXIS2_PLACEMENT_3D('',#24624,#20600,#20601);
#16292=AXIS2_PLACEMENT_3D('',#24626,#20602,#20603);
#16293=AXIS2_PLACEMENT_3D('',#24628,#20605,#20606);
#16294=AXIS2_PLACEMENT_3D('',#24630,#20607,#20608);
#16295=AXIS2_PLACEMENT_3D('',#24631,#20609,#20610);
#16296=AXIS2_PLACEMENT_3D('',#24633,#20612,#20613);
#16297=AXIS2_PLACEMENT_3D('',#24635,#20614,#20615);
#16298=AXIS2_PLACEMENT_3D('',#24637,#20616,#20617);
#16299=AXIS2_PLACEMENT_3D('',#24638,#20618,#20619);
#16300=AXIS2_PLACEMENT_3D('',#24640,#20620,#20621);
#16301=AXIS2_PLACEMENT_3D('',#24642,#20623,#20624);
#16302=AXIS2_PLACEMENT_3D('',#24644,#20625,#20626);
#16303=AXIS2_PLACEMENT_3D('',#24645,#20627,#20628);
#16304=AXIS2_PLACEMENT_3D('',#24647,#20630,#20631);
#16305=AXIS2_PLACEMENT_3D('',#24648,#20632,#20633);
#16306=AXIS2_PLACEMENT_3D('',#24649,#20634,#20635);
#16307=AXIS2_PLACEMENT_3D('',#24650,#20636,#20637);
#16308=AXIS2_PLACEMENT_3D('',#24651,#20638,#20639);
#16309=AXIS2_PLACEMENT_3D('',#24652,#20640,#20641);
#16310=AXIS2_PLACEMENT_3D('',#24653,#20642,#20643);
#16311=AXIS2_PLACEMENT_3D('',#24654,#20644,#20645);
#16312=AXIS2_PLACEMENT_3D('',#24655,#20646,#20647);
#16313=AXIS2_PLACEMENT_3D('',#24656,#20648,#20649);
#16314=AXIS2_PLACEMENT_3D('',#24657,#20650,#20651);
#16315=AXIS2_PLACEMENT_3D('',#24658,#20652,#20653);
#16316=AXIS2_PLACEMENT_3D('',#24659,#20654,#20655);
#16317=AXIS2_PLACEMENT_3D('',#24660,#20656,#20657);
#16318=AXIS2_PLACEMENT_3D('',#24661,#20658,#20659);
#16319=AXIS2_PLACEMENT_3D('',#24662,#20660,#20661);
#16320=AXIS2_PLACEMENT_3D('',#24663,#20662,#20663);
#16321=AXIS2_PLACEMENT_3D('',#24664,#20664,#20665);
#16322=AXIS2_PLACEMENT_3D('',#24665,#20666,#20667);
#16323=AXIS2_PLACEMENT_3D('',#24666,#20668,#20669);
#16324=AXIS2_PLACEMENT_3D('',#24667,#20670,#20671);
#16325=AXIS2_PLACEMENT_3D('',#24668,#20672,#20673);
#16326=AXIS2_PLACEMENT_3D('',#24669,#20674,#20675);
#16327=AXIS2_PLACEMENT_3D('',#24670,#20676,#20677);
#16328=AXIS2_PLACEMENT_3D('',#24671,#20678,#20679);
#16329=AXIS2_PLACEMENT_3D('',#24672,#20680,#20681);
#16330=AXIS2_PLACEMENT_3D('',#24673,#20682,#20683);
#16331=AXIS2_PLACEMENT_3D('',#24674,#20684,#20685);
#16332=AXIS2_PLACEMENT_3D('',#24675,#20686,#20687);
#16333=AXIS2_PLACEMENT_3D('',#24676,#20688,#20689);
#16334=AXIS2_PLACEMENT_3D('',#24677,#20690,#20691);
#16335=AXIS2_PLACEMENT_3D('',#24678,#20692,#20693);
#16336=AXIS2_PLACEMENT_3D('',#24679,#20694,#20695);
#16337=AXIS2_PLACEMENT_3D('',#24680,#20696,#20697);
#16338=AXIS2_PLACEMENT_3D('',#24681,#20698,#20699);
#16339=AXIS2_PLACEMENT_3D('',#24682,#20700,#20701);
#16340=AXIS2_PLACEMENT_3D('',#24683,#20702,#20703);
#16341=AXIS2_PLACEMENT_3D('',#24684,#20704,#20705);
#16342=AXIS2_PLACEMENT_3D('',#24685,#20706,#20707);
#16343=AXIS2_PLACEMENT_3D('',#24686,#20708,#20709);
#16344=AXIS2_PLACEMENT_3D('',#24687,#20710,#20711);
#16345=AXIS2_PLACEMENT_3D('',#24688,#20712,#20713);
#16346=AXIS2_PLACEMENT_3D('',#24689,#20714,#20715);
#16347=AXIS2_PLACEMENT_3D('',#24690,#20716,#20717);
#16348=AXIS2_PLACEMENT_3D('',#24691,#20718,#20719);
#16349=AXIS2_PLACEMENT_3D('',#24692,#20720,#20721);
#16350=AXIS2_PLACEMENT_3D('',#24693,#20722,#20723);
#16351=AXIS2_PLACEMENT_3D('',#24694,#20724,#20725);
#16352=AXIS2_PLACEMENT_3D('',#24695,#20726,#20727);
#16353=AXIS2_PLACEMENT_3D('',#24696,#20728,#20729);
#16354=AXIS2_PLACEMENT_3D('',#24697,#20730,#20731);
#16355=AXIS2_PLACEMENT_3D('',#24698,#20732,#20733);
#16356=AXIS2_PLACEMENT_3D('',#24699,#20734,#20735);
#16357=AXIS2_PLACEMENT_3D('',#24700,#20736,#20737);
#16358=AXIS2_PLACEMENT_3D('',#24701,#20738,#20739);
#16359=AXIS2_PLACEMENT_3D('',#24702,#20740,#20741);
#16360=AXIS2_PLACEMENT_3D('',#24703,#20742,#20743);
#16361=AXIS2_PLACEMENT_3D('',#24704,#20744,#20745);
#16362=AXIS2_PLACEMENT_3D('',#24705,#20746,#20747);
#16363=AXIS2_PLACEMENT_3D('',#24706,#20748,#20749);
#16364=AXIS2_PLACEMENT_3D('',#24707,#20750,#20751);
#16365=AXIS2_PLACEMENT_3D('',#24708,#20752,#20753);
#16366=AXIS2_PLACEMENT_3D('',#24709,#20754,#20755);
#16367=AXIS2_PLACEMENT_3D('',#24710,#20756,#20757);
#16368=AXIS2_PLACEMENT_3D('',#24711,#20758,#20759);
#16369=AXIS2_PLACEMENT_3D('',#24712,#20760,#20761);
#16370=AXIS2_PLACEMENT_3D('',#24713,#20762,#20763);
#16371=AXIS2_PLACEMENT_3D('',#24714,#20764,#20765);
#16372=AXIS2_PLACEMENT_3D('',#24715,#20766,#20767);
#16373=AXIS2_PLACEMENT_3D('',#24716,#20768,#20769);
#16374=AXIS2_PLACEMENT_3D('',#24717,#20770,#20771);
#16375=AXIS2_PLACEMENT_3D('',#24718,#20772,#20773);
#16376=AXIS2_PLACEMENT_3D('',#24719,#20774,#20775);
#16377=AXIS2_PLACEMENT_3D('',#24720,#20776,#20777);
#16378=AXIS2_PLACEMENT_3D('',#24721,#20778,#20779);
#16379=AXIS2_PLACEMENT_3D('',#24722,#20780,#20781);
#16380=AXIS2_PLACEMENT_3D('',#24723,#20782,#20783);
#16381=AXIS2_PLACEMENT_3D('',#24724,#20784,#20785);
#16382=AXIS2_PLACEMENT_3D('',#24725,#20786,#20787);
#16383=AXIS2_PLACEMENT_3D('',#24726,#20788,#20789);
#16384=AXIS2_PLACEMENT_3D('',#24727,#20790,#20791);
#16385=AXIS2_PLACEMENT_3D('',#24729,#20792,#20793);
#16386=AXIS2_PLACEMENT_3D('',#24731,#20794,#20795);
#16387=AXIS2_PLACEMENT_3D('',#24732,#20796,#20797);
#16388=AXIS2_PLACEMENT_3D('',#24734,#20798,#20799);
#16389=AXIS2_PLACEMENT_3D('',#24736,#20800,#20801);
#16390=AXIS2_PLACEMENT_3D('',#24737,#20802,#20803);
#16391=AXIS2_PLACEMENT_3D('',#24739,#20805,#20806);
#16392=AXIS2_PLACEMENT_3D('',#24742,#20808,#20809);
#16393=AXIS2_PLACEMENT_3D('',#24743,#20810,#20811);
#16394=AXIS2_PLACEMENT_3D('',#24745,#20812,#20813);
#16395=AXIS2_PLACEMENT_3D('',#24746,#20814,#20815);
#16396=AXIS2_PLACEMENT_3D('',#24748,#20816,#20817);
#16397=AXIS2_PLACEMENT_3D('',#24750,#20818,#20819);
#16398=AXIS2_PLACEMENT_3D('',#24751,#20820,#20821);
#16399=AXIS2_PLACEMENT_3D('',#24753,#20823,#20824);
#16400=AXIS2_PLACEMENT_3D('',#24756,#20826,#20827);
#16401=AXIS2_PLACEMENT_3D('',#24757,#20828,#20829);
#16402=AXIS2_PLACEMENT_3D('',#24759,#20830,#20831);
#16403=AXIS2_PLACEMENT_3D('',#24761,#20833,#20834);
#16404=AXIS2_PLACEMENT_3D('',#24762,#20835,#20836);
#16405=AXIS2_PLACEMENT_3D('',#24763,#20837,#20838);
#16406=AXIS2_PLACEMENT_3D('',#24764,#20839,#20840);
#16407=AXIS2_PLACEMENT_3D('',#24766,#20841,#20842);
#16408=AXIS2_PLACEMENT_3D('',#24769,#20844,#20845);
#16409=AXIS2_PLACEMENT_3D('',#24770,#20846,#20847);
#16410=AXIS2_PLACEMENT_3D('',#24772,#20848,#20849);
#16411=AXIS2_PLACEMENT_3D('',#24775,#20851,#20852);
#16412=AXIS2_PLACEMENT_3D('',#24776,#20853,#20854);
#16413=AXIS2_PLACEMENT_3D('',#24777,#20855,#20856);
#16414=AXIS2_PLACEMENT_3D('',#24778,#20857,#20858);
#16415=AXIS2_PLACEMENT_3D('',#24779,#20859,#20860);
#16416=AXIS2_PLACEMENT_3D('',#24781,#20861,#20862);
#16417=AXIS2_PLACEMENT_3D('',#24784,#20864,#20865);
#16418=AXIS2_PLACEMENT_3D('',#24785,#20866,#20867);
#16419=AXIS2_PLACEMENT_3D('',#24787,#20868,#20869);
#16420=AXIS2_PLACEMENT_3D('',#24790,#20871,#20872);
#16421=AXIS2_PLACEMENT_3D('',#24791,#20873,#20874);
#16422=AXIS2_PLACEMENT_3D('',#24792,#20875,#20876);
#16423=AXIS2_PLACEMENT_3D('',#24793,#20877,#20878);
#16424=AXIS2_PLACEMENT_3D('',#24794,#20879,#20880);
#16425=AXIS2_PLACEMENT_3D('',#24796,#20881,#20882);
#16426=AXIS2_PLACEMENT_3D('',#24799,#20884,#20885);
#16427=AXIS2_PLACEMENT_3D('',#24800,#20886,#20887);
#16428=AXIS2_PLACEMENT_3D('',#24802,#20888,#20889);
#16429=AXIS2_PLACEMENT_3D('',#24805,#20891,#20892);
#16430=AXIS2_PLACEMENT_3D('',#24806,#20893,#20894);
#16431=AXIS2_PLACEMENT_3D('',#24807,#20895,#20896);
#16432=AXIS2_PLACEMENT_3D('',#24808,#20897,#20898);
#16433=AXIS2_PLACEMENT_3D('',#24809,#20899,#20900);
#16434=AXIS2_PLACEMENT_3D('',#24811,#20901,#20902);
#16435=AXIS2_PLACEMENT_3D('',#24814,#20904,#20905);
#16436=AXIS2_PLACEMENT_3D('',#24815,#20906,#20907);
#16437=AXIS2_PLACEMENT_3D('',#24817,#20908,#20909);
#16438=AXIS2_PLACEMENT_3D('',#24820,#20911,#20912);
#16439=AXIS2_PLACEMENT_3D('',#24821,#20913,#20914);
#16440=AXIS2_PLACEMENT_3D('',#24822,#20915,#20916);
#16441=AXIS2_PLACEMENT_3D('',#24823,#20917,#20918);
#16442=AXIS2_PLACEMENT_3D('',#24824,#20919,#20920);
#16443=AXIS2_PLACEMENT_3D('',#24826,#20921,#20922);
#16444=AXIS2_PLACEMENT_3D('',#24829,#20924,#20925);
#16445=AXIS2_PLACEMENT_3D('',#24830,#20926,#20927);
#16446=AXIS2_PLACEMENT_3D('',#24831,#20928,#20929);
#16447=AXIS2_PLACEMENT_3D('',#24833,#20930,#20931);
#16448=AXIS2_PLACEMENT_3D('',#24836,#20933,#20934);
#16449=AXIS2_PLACEMENT_3D('',#24837,#20935,#20936);
#16450=AXIS2_PLACEMENT_3D('',#24839,#20937,#20938);
#16451=AXIS2_PLACEMENT_3D('',#24842,#20940,#20941);
#16452=AXIS2_PLACEMENT_3D('',#24843,#20942,#20943);
#16453=AXIS2_PLACEMENT_3D('',#24844,#20944,#20945);
#16454=AXIS2_PLACEMENT_3D('',#24845,#20946,#20947);
#16455=AXIS2_PLACEMENT_3D('',#24846,#20948,#20949);
#16456=AXIS2_PLACEMENT_3D('',#24847,#20950,#20951);
#16457=AXIS2_PLACEMENT_3D('',#24848,#20952,#20953);
#16458=AXIS2_PLACEMENT_3D('',#24849,#20954,#20955);
#16459=AXIS2_PLACEMENT_3D('',#24850,#20956,#20957);
#16460=AXIS2_PLACEMENT_3D('',#24851,#20958,#20959);
#16461=AXIS2_PLACEMENT_3D('',#24852,#20960,#20961);
#16462=AXIS2_PLACEMENT_3D('',#24853,#20962,#20963);
#16463=AXIS2_PLACEMENT_3D('',#24854,#20964,#20965);
#16464=AXIS2_PLACEMENT_3D('',#24855,#20966,#20967);
#16465=AXIS2_PLACEMENT_3D('',#24856,#20968,#20969);
#16466=AXIS2_PLACEMENT_3D('',#24857,#20970,#20971);
#16467=AXIS2_PLACEMENT_3D('',#24858,#20972,#20973);
#16468=DIRECTION('axis',(0.,0.,1.));
#16469=DIRECTION('refdir',(1.,0.,0.));
#16470=DIRECTION('axis',(0.,0.,1.));
#16471=DIRECTION('refdir',(1.,0.,0.));
#16472=DIRECTION('axis',(0.,0.,1.));
#16473=DIRECTION('refdir',(1.,0.,0.));
#16474=DIRECTION('center_axis',(0.,0.,1.));
#16475=DIRECTION('ref_axis',(1.,0.,0.));
#16476=DIRECTION('center_axis',(0.,0.,1.));
#16477=DIRECTION('ref_axis',(1.,0.,0.));
#16478=DIRECTION('',(0.,0.,1.));
#16479=DIRECTION('center_axis',(0.,0.,-1.));
#16480=DIRECTION('ref_axis',(1.,0.,0.));
#16481=DIRECTION('center_axis',(0.,0.,1.));
#16482=DIRECTION('ref_axis',(1.,0.,0.));
#16483=DIRECTION('center_axis',(0.,0.,1.));
#16484=DIRECTION('ref_axis',(1.,0.,0.));
#16485=DIRECTION('',(0.,0.,1.));
#16486=DIRECTION('center_axis',(0.,0.,-1.));
#16487=DIRECTION('ref_axis',(1.,0.,0.));
#16488=DIRECTION('center_axis',(0.,0.,1.));
#16489=DIRECTION('ref_axis',(1.,0.,0.));
#16490=DIRECTION('center_axis',(0.,0.,1.));
#16491=DIRECTION('ref_axis',(1.,0.,0.));
#16492=DIRECTION('',(0.,0.,1.));
#16493=DIRECTION('center_axis',(0.,0.,-1.));
#16494=DIRECTION('ref_axis',(1.,0.,0.));
#16495=DIRECTION('center_axis',(0.,0.,1.));
#16496=DIRECTION('ref_axis',(1.,0.,0.));
#16497=DIRECTION('center_axis',(0.,0.,1.));
#16498=DIRECTION('ref_axis',(1.,0.,0.));
#16499=DIRECTION('',(0.,0.,1.));
#16500=DIRECTION('center_axis',(0.,0.,-1.));
#16501=DIRECTION('ref_axis',(1.,0.,0.));
#16502=DIRECTION('center_axis',(0.,0.,1.));
#16503=DIRECTION('ref_axis',(1.,0.,0.));
#16504=DIRECTION('center_axis',(0.,0.,1.));
#16505=DIRECTION('ref_axis',(1.,0.,0.));
#16506=DIRECTION('',(0.,0.,1.));
#16507=DIRECTION('center_axis',(0.,0.,-1.));
#16508=DIRECTION('ref_axis',(1.,0.,0.));
#16509=DIRECTION('center_axis',(0.,0.,1.));
#16510=DIRECTION('ref_axis',(1.,0.,0.));
#16511=DIRECTION('center_axis',(0.,0.,1.));
#16512=DIRECTION('ref_axis',(1.,0.,0.));
#16513=DIRECTION('',(0.,0.,1.));
#16514=DIRECTION('center_axis',(0.,0.,-1.));
#16515=DIRECTION('ref_axis',(1.,0.,0.));
#16516=DIRECTION('center_axis',(0.,0.,1.));
#16517=DIRECTION('ref_axis',(1.,0.,0.));
#16518=DIRECTION('center_axis',(0.,0.,1.));
#16519=DIRECTION('ref_axis',(1.,0.,0.));
#16520=DIRECTION('',(0.,0.,1.));
#16521=DIRECTION('center_axis',(0.,0.,-1.));
#16522=DIRECTION('ref_axis',(1.,0.,0.));
#16523=DIRECTION('center_axis',(0.,0.,1.));
#16524=DIRECTION('ref_axis',(1.,0.,0.));
#16525=DIRECTION('center_axis',(0.,0.,1.));
#16526=DIRECTION('ref_axis',(1.,0.,0.));
#16527=DIRECTION('',(0.,0.,1.));
#16528=DIRECTION('center_axis',(0.,0.,-1.));
#16529=DIRECTION('ref_axis',(1.,0.,0.));
#16530=DIRECTION('center_axis',(0.,1.,0.));
#16531=DIRECTION('ref_axis',(-1.,0.,0.));
#16532=DIRECTION('',(-1.,0.,0.));
#16533=DIRECTION('',(0.,0.,1.));
#16534=DIRECTION('',(-1.,0.,0.));
#16535=DIRECTION('',(0.,0.,1.));
#16536=DIRECTION('center_axis',(1.,0.,0.));
#16537=DIRECTION('ref_axis',(0.,1.,0.));
#16538=DIRECTION('',(0.,1.,0.));
#16539=DIRECTION('',(0.,1.,0.));
#16540=DIRECTION('',(0.,0.,1.));
#16541=DIRECTION('center_axis',(0.,-1.,0.));
#16542=DIRECTION('ref_axis',(1.,0.,0.));
#16543=DIRECTION('',(1.,0.,0.));
#16544=DIRECTION('',(1.,0.,0.));
#16545=DIRECTION('',(0.,0.,1.));
#16546=DIRECTION('center_axis',(-1.,0.,0.));
#16547=DIRECTION('ref_axis',(0.,-1.,0.));
#16548=DIRECTION('',(0.,-1.,0.));
#16549=DIRECTION('',(0.,-1.,0.));
#16550=DIRECTION('center_axis',(0.,0.,1.));
#16551=DIRECTION('ref_axis',(1.,0.,0.));
#16552=DIRECTION('center_axis',(0.,0.,1.));
#16553=DIRECTION('ref_axis',(1.,0.,0.));
#16554=DIRECTION('axis',(0.,0.,1.));
#16555=DIRECTION('refdir',(1.,0.,0.));
#16556=DIRECTION('center_axis',(0.,1.,0.));
#16557=DIRECTION('ref_axis',(-1.,0.,0.));
#16558=DIRECTION('',(-1.,0.,0.));
#16559=DIRECTION('',(0.,0.,1.));
#16560=DIRECTION('',(-1.,0.,0.));
#16561=DIRECTION('',(0.,0.,1.));
#16562=DIRECTION('center_axis',(1.,0.,0.));
#16563=DIRECTION('ref_axis',(0.,1.,0.));
#16564=DIRECTION('',(0.,1.,0.));
#16565=DIRECTION('',(0.,1.,0.));
#16566=DIRECTION('',(0.,0.,1.));
#16567=DIRECTION('center_axis',(0.,-1.,0.));
#16568=DIRECTION('ref_axis',(1.,0.,0.));
#16569=DIRECTION('',(1.,0.,0.));
#16570=DIRECTION('',(1.,0.,0.));
#16571=DIRECTION('',(0.,0.,1.));
#16572=DIRECTION('center_axis',(-1.,0.,0.));
#16573=DIRECTION('ref_axis',(0.,-1.,0.));
#16574=DIRECTION('',(0.,-1.,0.));
#16575=DIRECTION('',(0.,-1.,0.));
#16576=DIRECTION('center_axis',(0.,0.,1.));
#16577=DIRECTION('ref_axis',(1.,0.,0.));
#16578=DIRECTION('center_axis',(0.,0.,1.));
#16579=DIRECTION('ref_axis',(1.,0.,0.));
#16580=DIRECTION('axis',(0.,0.,1.));
#16581=DIRECTION('refdir',(1.,0.,0.));
#16582=DIRECTION('center_axis',(0.,1.,0.));
#16583=DIRECTION('ref_axis',(-1.,0.,0.));
#16584=DIRECTION('',(-1.,0.,0.));
#16585=DIRECTION('',(0.,0.,1.));
#16586=DIRECTION('',(-1.,0.,0.));
#16587=DIRECTION('',(0.,0.,1.));
#16588=DIRECTION('center_axis',(1.,0.,0.));
#16589=DIRECTION('ref_axis',(0.,1.,0.));
#16590=DIRECTION('',(0.,1.,0.));
#16591=DIRECTION('',(0.,1.,0.));
#16592=DIRECTION('',(0.,0.,1.));
#16593=DIRECTION('center_axis',(0.,-1.,0.));
#16594=DIRECTION('ref_axis',(1.,0.,0.));
#16595=DIRECTION('',(1.,0.,0.));
#16596=DIRECTION('',(1.,0.,0.));
#16597=DIRECTION('',(0.,0.,1.));
#16598=DIRECTION('center_axis',(-1.,0.,0.));
#16599=DIRECTION('ref_axis',(0.,-1.,0.));
#16600=DIRECTION('',(0.,-1.,0.));
#16601=DIRECTION('',(0.,-1.,0.));
#16602=DIRECTION('center_axis',(0.,0.,1.));
#16603=DIRECTION('ref_axis',(1.,0.,0.));
#16604=DIRECTION('center_axis',(0.,0.,1.));
#16605=DIRECTION('ref_axis',(1.,0.,0.));
#16606=DIRECTION('axis',(0.,0.,1.));
#16607=DIRECTION('refdir',(1.,0.,0.));
#16608=DIRECTION('center_axis',(1.,0.,0.));
#16609=DIRECTION('ref_axis',(0.,0.,-1.));
#16610=DIRECTION('center_axis',(1.,0.,0.));
#16611=DIRECTION('ref_axis',(0.,0.,-1.));
#16612=DIRECTION('',(1.,0.,0.));
#16613=DIRECTION('center_axis',(-1.,0.,0.));
#16614=DIRECTION('ref_axis',(0.,0.,-1.));
#16615=DIRECTION('center_axis',(1.,0.,0.));
#16616=DIRECTION('ref_axis',(0.,0.,-1.));
#16617=DIRECTION('center_axis',(1.,0.,0.));
#16618=DIRECTION('ref_axis',(0.,0.,-1.));
#16619=DIRECTION('',(1.,0.,0.));
#16620=DIRECTION('center_axis',(-1.,0.,0.));
#16621=DIRECTION('ref_axis',(0.,0.,-1.));
#16622=DIRECTION('center_axis',(1.,0.,0.));
#16623=DIRECTION('ref_axis',(0.,0.,-1.));
#16624=DIRECTION('center_axis',(1.,0.,0.));
#16625=DIRECTION('ref_axis',(0.,0.,-1.));
#16626=DIRECTION('',(1.,0.,0.));
#16627=DIRECTION('center_axis',(-1.,0.,0.));
#16628=DIRECTION('ref_axis',(0.,0.,-1.));
#16629=DIRECTION('center_axis',(1.,0.,0.));
#16630=DIRECTION('ref_axis',(0.,0.,-1.));
#16631=DIRECTION('center_axis',(1.,0.,0.));
#16632=DIRECTION('ref_axis',(0.,0.,-1.));
#16633=DIRECTION('',(1.,0.,0.));
#16634=DIRECTION('center_axis',(-1.,0.,0.));
#16635=DIRECTION('ref_axis',(0.,0.,-1.));
#16636=DIRECTION('center_axis',(1.,0.,0.));
#16637=DIRECTION('ref_axis',(0.,0.,-1.));
#16638=DIRECTION('center_axis',(1.,0.,0.));
#16639=DIRECTION('ref_axis',(0.,0.,-1.));
#16640=DIRECTION('',(1.,0.,0.));
#16641=DIRECTION('center_axis',(-1.,0.,0.));
#16642=DIRECTION('ref_axis',(0.,0.,-1.));
#16643=DIRECTION('center_axis',(0.,0.,1.));
#16644=DIRECTION('ref_axis',(1.,0.,0.));
#16645=DIRECTION('center_axis',(0.,0.,1.));
#16646=DIRECTION('ref_axis',(1.,0.,0.));
#16647=DIRECTION('',(0.,0.,1.));
#16648=DIRECTION('center_axis',(0.,0.,-1.));
#16649=DIRECTION('ref_axis',(1.,0.,0.));
#16650=DIRECTION('center_axis',(0.,0.,1.));
#16651=DIRECTION('ref_axis',(1.,0.,0.));
#16652=DIRECTION('center_axis',(0.,0.,1.));
#16653=DIRECTION('ref_axis',(1.,0.,0.));
#16654=DIRECTION('',(0.,0.,1.));
#16655=DIRECTION('center_axis',(0.,0.,-1.));
#16656=DIRECTION('ref_axis',(1.,0.,0.));
#16657=DIRECTION('center_axis',(0.,0.,1.));
#16658=DIRECTION('ref_axis',(1.,0.,0.));
#16659=DIRECTION('center_axis',(0.,0.,1.));
#16660=DIRECTION('ref_axis',(1.,0.,0.));
#16661=DIRECTION('',(0.,0.,1.));
#16662=DIRECTION('center_axis',(0.,0.,-1.));
#16663=DIRECTION('ref_axis',(1.,0.,0.));
#16664=DIRECTION('center_axis',(0.,0.,1.));
#16665=DIRECTION('ref_axis',(1.,0.,0.));
#16666=DIRECTION('center_axis',(0.,0.,1.));
#16667=DIRECTION('ref_axis',(1.,0.,0.));
#16668=DIRECTION('',(0.,0.,1.));
#16669=DIRECTION('center_axis',(0.,0.,-1.));
#16670=DIRECTION('ref_axis',(1.,0.,0.));
#16671=DIRECTION('center_axis',(0.,0.,1.));
#16672=DIRECTION('ref_axis',(1.,0.,0.));
#16673=DIRECTION('',(0.,-1.,0.));
#16674=DIRECTION('',(-1.,0.,0.));
#16675=DIRECTION('',(0.,-1.,0.));
#16676=DIRECTION('',(1.,0.,0.));
#16677=DIRECTION('center_axis',(0.,0.,1.));
#16678=DIRECTION('ref_axis',(1.,0.,0.));
#16679=DIRECTION('',(0.,1.,0.));
#16680=DIRECTION('',(1.,0.,0.));
#16681=DIRECTION('',(0.,1.,0.));
#16682=DIRECTION('',(-1.,0.,0.));
#16683=DIRECTION('center_axis',(1.,0.,0.));
#16684=DIRECTION('ref_axis',(0.,1.,0.));
#16685=DIRECTION('',(0.,1.,0.));
#16686=DIRECTION('',(0.,0.,1.));
#16687=DIRECTION('',(0.,0.,1.));
#16688=DIRECTION('center_axis',(-1.,0.,0.));
#16689=DIRECTION('ref_axis',(0.,-1.,0.));
#16690=DIRECTION('',(0.,-1.,0.));
#16691=DIRECTION('',(0.,0.,1.));
#16692=DIRECTION('',(0.,0.,1.));
#16693=DIRECTION('center_axis',(0.,1.,0.));
#16694=DIRECTION('ref_axis',(-1.,0.,0.));
#16695=DIRECTION('',(0.,0.,1.));
#16696=DIRECTION('',(-1.,0.,0.));
#16697=DIRECTION('',(0.,0.,1.));
#16698=DIRECTION('',(-1.,0.,0.));
#16699=DIRECTION('center_axis',(0.,-1.,0.));
#16700=DIRECTION('ref_axis',(1.,0.,0.));
#16701=DIRECTION('center_axis',(-1.,0.,0.));
#16702=DIRECTION('ref_axis',(0.,-1.,0.));
#16703=DIRECTION('',(0.,0.,1.));
#16704=DIRECTION('',(0.,-1.,0.));
#16705=DIRECTION('center_axis',(1.,0.,0.));
#16706=DIRECTION('ref_axis',(0.,0.,-1.));
#16707=DIRECTION('center_axis',(1.,0.,0.));
#16708=DIRECTION('ref_axis',(0.,0.,-1.));
#16709=DIRECTION('center_axis',(0.,1.,0.));
#16710=DIRECTION('ref_axis',(1.,0.,0.));
#16711=DIRECTION('center_axis',(0.,1.,0.));
#16712=DIRECTION('ref_axis',(1.,0.,0.));
#16713=DIRECTION('',(0.,1.,0.));
#16714=DIRECTION('center_axis',(1.,0.,0.));
#16715=DIRECTION('ref_axis',(0.,0.,-1.));
#16716=DIRECTION('',(1.,0.,0.));
#16717=DIRECTION('center_axis',(-1.,0.,0.));
#16718=DIRECTION('ref_axis',(0.,0.,-1.));
#16719=DIRECTION('center_axis',(1.,0.,0.));
#16720=DIRECTION('ref_axis',(0.,0.,-1.));
#16721=DIRECTION('',(1.,0.,0.));
#16722=DIRECTION('center_axis',(-1.,0.,0.));
#16723=DIRECTION('ref_axis',(0.,0.,-1.));
#16724=DIRECTION('center_axis',(1.,0.,0.));
#16725=DIRECTION('ref_axis',(0.,1.,0.));
#16726=DIRECTION('',(0.,1.,0.));
#16727=DIRECTION('',(0.,0.,1.));
#16728=DIRECTION('center_axis',(0.,-1.,0.));
#16729=DIRECTION('ref_axis',(1.,0.,0.));
#16730=DIRECTION('',(1.,0.,0.));
#16731=DIRECTION('',(1.,0.,0.));
#16732=DIRECTION('center_axis',(0.,0.,1.));
#16733=DIRECTION('ref_axis',(1.,0.,0.));
#16734=DIRECTION('center_axis',(0.,0.,1.));
#16735=DIRECTION('ref_axis',(1.,0.,0.));
#16736=DIRECTION('axis',(0.,0.,1.));
#16737=DIRECTION('refdir',(1.,0.,0.));
#16738=DIRECTION('center_axis',(1.,0.,0.));
#16739=DIRECTION('ref_axis',(0.,0.,-1.));
#16740=DIRECTION('center_axis',(1.,0.,0.));
#16741=DIRECTION('ref_axis',(0.,0.,-1.));
#16742=DIRECTION('',(1.,0.,0.));
#16743=DIRECTION('center_axis',(-1.,0.,0.));
#16744=DIRECTION('ref_axis',(0.,0.,-1.));
#16745=DIRECTION('center_axis',(1.,0.,0.));
#16746=DIRECTION('ref_axis',(0.,0.,-1.));
#16747=DIRECTION('center_axis',(1.,0.,0.));
#16748=DIRECTION('ref_axis',(0.,0.,-1.));
#16749=DIRECTION('',(1.,0.,0.));
#16750=DIRECTION('center_axis',(-1.,0.,0.));
#16751=DIRECTION('ref_axis',(0.,0.,-1.));
#16752=DIRECTION('center_axis',(1.,0.,0.));
#16753=DIRECTION('ref_axis',(0.,0.,-1.));
#16754=DIRECTION('center_axis',(1.,0.,0.));
#16755=DIRECTION('ref_axis',(0.,0.,-1.));
#16756=DIRECTION('',(1.,0.,0.));
#16757=DIRECTION('center_axis',(-1.,0.,0.));
#16758=DIRECTION('ref_axis',(0.,0.,-1.));
#16759=DIRECTION('center_axis',(1.,0.,0.));
#16760=DIRECTION('ref_axis',(0.,0.,-1.));
#16761=DIRECTION('center_axis',(1.,0.,0.));
#16762=DIRECTION('ref_axis',(0.,0.,-1.));
#16763=DIRECTION('',(1.,0.,0.));
#16764=DIRECTION('center_axis',(-1.,0.,0.));
#16765=DIRECTION('ref_axis',(0.,0.,-1.));
#16766=DIRECTION('center_axis',(1.,0.,0.));
#16767=DIRECTION('ref_axis',(0.,0.,-1.));
#16768=DIRECTION('center_axis',(1.,0.,0.));
#16769=DIRECTION('ref_axis',(0.,0.,-1.));
#16770=DIRECTION('',(-1.,0.,0.));
#16771=DIRECTION('center_axis',(-1.,0.,0.));
#16772=DIRECTION('ref_axis',(0.,0.,-1.));
#16773=DIRECTION('center_axis',(1.,0.,0.));
#16774=DIRECTION('ref_axis',(0.,0.,-1.));
#16775=DIRECTION('center_axis',(-1.,0.,0.));
#16776=DIRECTION('ref_axis',(0.,0.,-1.));
#16777=DIRECTION('center_axis',(1.,0.,0.));
#16778=DIRECTION('ref_axis',(0.,0.,-1.));
#16779=DIRECTION('',(-1.,0.,0.));
#16780=DIRECTION('center_axis',(-1.,0.,0.));
#16781=DIRECTION('ref_axis',(0.,0.,-1.));
#16782=DIRECTION('center_axis',(1.,0.,0.));
#16783=DIRECTION('ref_axis',(0.,0.,-1.));
#16784=DIRECTION('center_axis',(1.,0.,0.));
#16785=DIRECTION('ref_axis',(0.,0.,-1.));
#16786=DIRECTION('',(-1.,0.,0.));
#16787=DIRECTION('center_axis',(1.,0.,0.));
#16788=DIRECTION('ref_axis',(0.,0.,-1.));
#16789=DIRECTION('center_axis',(1.,0.,0.));
#16790=DIRECTION('ref_axis',(0.,0.,-1.));
#16791=DIRECTION('center_axis',(1.,0.,0.));
#16792=DIRECTION('ref_axis',(0.,0.,-1.));
#16793=DIRECTION('axis',(0.,0.,1.));
#16794=DIRECTION('refdir',(1.,0.,0.));
#16795=DIRECTION('center_axis',(1.,0.,0.));
#16796=DIRECTION('ref_axis',(0.,0.,-1.));
#16797=DIRECTION('center_axis',(1.,0.,0.));
#16798=DIRECTION('ref_axis',(0.,0.,-1.));
#16799=DIRECTION('',(1.,0.,0.));
#16800=DIRECTION('center_axis',(-1.,0.,0.));
#16801=DIRECTION('ref_axis',(0.,0.,-1.));
#16802=DIRECTION('center_axis',(1.,0.,0.));
#16803=DIRECTION('ref_axis',(0.,0.,-1.));
#16804=DIRECTION('center_axis',(1.,0.,0.));
#16805=DIRECTION('ref_axis',(0.,0.,-1.));
#16806=DIRECTION('',(1.,0.,0.));
#16807=DIRECTION('center_axis',(-1.,0.,0.));
#16808=DIRECTION('ref_axis',(0.,0.,-1.));
#16809=DIRECTION('center_axis',(1.,0.,0.));
#16810=DIRECTION('ref_axis',(0.,0.,-1.));
#16811=DIRECTION('center_axis',(1.,0.,0.));
#16812=DIRECTION('ref_axis',(0.,0.,-1.));
#16813=DIRECTION('',(1.,0.,0.));
#16814=DIRECTION('center_axis',(-1.,0.,0.));
#16815=DIRECTION('ref_axis',(0.,0.,-1.));
#16816=DIRECTION('center_axis',(1.,0.,0.));
#16817=DIRECTION('ref_axis',(0.,0.,-1.));
#16818=DIRECTION('center_axis',(1.,0.,0.));
#16819=DIRECTION('ref_axis',(0.,0.,-1.));
#16820=DIRECTION('',(1.,0.,0.));
#16821=DIRECTION('center_axis',(-1.,0.,0.));
#16822=DIRECTION('ref_axis',(0.,0.,-1.));
#16823=DIRECTION('center_axis',(1.,0.,0.));
#16824=DIRECTION('ref_axis',(0.,0.,-1.));
#16825=DIRECTION('center_axis',(1.,0.,0.));
#16826=DIRECTION('ref_axis',(0.,0.,-1.));
#16827=DIRECTION('',(-1.,0.,0.));
#16828=DIRECTION('center_axis',(1.,0.,0.));
#16829=DIRECTION('ref_axis',(0.,0.,-1.));
#16830=DIRECTION('center_axis',(1.,0.,0.));
#16831=DIRECTION('ref_axis',(0.,0.,-1.));
#16832=DIRECTION('center_axis',(-1.,0.,0.));
#16833=DIRECTION('ref_axis',(0.,0.,-1.));
#16834=DIRECTION('center_axis',(1.,0.,0.));
#16835=DIRECTION('ref_axis',(0.,0.,-1.));
#16836=DIRECTION('center_axis',(-1.,0.,0.));
#16837=DIRECTION('ref_axis',(0.,0.,-1.));
#16838=DIRECTION('',(-1.,0.,0.));
#16839=DIRECTION('center_axis',(1.,0.,0.));
#16840=DIRECTION('ref_axis',(0.,0.,-1.));
#16841=DIRECTION('center_axis',(1.,0.,0.));
#16842=DIRECTION('ref_axis',(0.,0.,-1.));
#16843=DIRECTION('',(-1.,0.,0.));
#16844=DIRECTION('center_axis',(1.,0.,0.));
#16845=DIRECTION('ref_axis',(0.,0.,-1.));
#16846=DIRECTION('center_axis',(1.,0.,0.));
#16847=DIRECTION('ref_axis',(0.,0.,-1.));
#16848=DIRECTION('center_axis',(1.,0.,0.));
#16849=DIRECTION('ref_axis',(0.,0.,-1.));
#16850=DIRECTION('axis',(0.,0.,1.));
#16851=DIRECTION('refdir',(1.,0.,0.));
#16852=DIRECTION('center_axis',(1.,0.,0.));
#16853=DIRECTION('ref_axis',(0.,0.,-1.));
#16854=DIRECTION('center_axis',(1.,0.,0.));
#16855=DIRECTION('ref_axis',(0.,0.,-1.));
#16856=DIRECTION('',(1.,0.,0.));
#16857=DIRECTION('center_axis',(-1.,0.,0.));
#16858=DIRECTION('ref_axis',(0.,0.,-1.));
#16859=DIRECTION('center_axis',(1.,0.,0.));
#16860=DIRECTION('ref_axis',(0.,0.,-1.));
#16861=DIRECTION('center_axis',(1.,0.,0.));
#16862=DIRECTION('ref_axis',(0.,0.,-1.));
#16863=DIRECTION('',(1.,0.,0.));
#16864=DIRECTION('center_axis',(-1.,0.,0.));
#16865=DIRECTION('ref_axis',(0.,0.,-1.));
#16866=DIRECTION('center_axis',(1.,0.,0.));
#16867=DIRECTION('ref_axis',(0.,0.,-1.));
#16868=DIRECTION('center_axis',(1.,0.,0.));
#16869=DIRECTION('ref_axis',(0.,0.,-1.));
#16870=DIRECTION('',(1.,0.,0.));
#16871=DIRECTION('center_axis',(-1.,0.,0.));
#16872=DIRECTION('ref_axis',(0.,0.,-1.));
#16873=DIRECTION('center_axis',(1.,0.,0.));
#16874=DIRECTION('ref_axis',(0.,0.,-1.));
#16875=DIRECTION('center_axis',(1.,0.,0.));
#16876=DIRECTION('ref_axis',(0.,0.,-1.));
#16877=DIRECTION('',(1.,0.,0.));
#16878=DIRECTION('center_axis',(-1.,0.,0.));
#16879=DIRECTION('ref_axis',(0.,0.,-1.));
#16880=DIRECTION('center_axis',(1.,0.,0.));
#16881=DIRECTION('ref_axis',(0.,0.,-1.));
#16882=DIRECTION('center_axis',(1.,0.,0.));
#16883=DIRECTION('ref_axis',(0.,0.,-1.));
#16884=DIRECTION('',(1.,0.,0.));
#16885=DIRECTION('center_axis',(-1.,0.,0.));
#16886=DIRECTION('ref_axis',(0.,0.,-1.));
#16887=DIRECTION('center_axis',(0.,0.,1.));
#16888=DIRECTION('ref_axis',(1.,0.,0.));
#16889=DIRECTION('center_axis',(0.,0.,1.));
#16890=DIRECTION('ref_axis',(1.,0.,0.));
#16891=DIRECTION('',(0.,0.,1.));
#16892=DIRECTION('center_axis',(0.,0.,-1.));
#16893=DIRECTION('ref_axis',(1.,0.,0.));
#16894=DIRECTION('center_axis',(0.,0.,1.));
#16895=DIRECTION('ref_axis',(1.,0.,0.));
#16896=DIRECTION('center_axis',(0.,0.,1.));
#16897=DIRECTION('ref_axis',(1.,0.,0.));
#16898=DIRECTION('',(0.,0.,1.));
#16899=DIRECTION('center_axis',(0.,0.,-1.));
#16900=DIRECTION('ref_axis',(1.,0.,0.));
#16901=DIRECTION('center_axis',(0.,0.,1.));
#16902=DIRECTION('ref_axis',(1.,0.,0.));
#16903=DIRECTION('center_axis',(0.,0.,1.));
#16904=DIRECTION('ref_axis',(1.,0.,0.));
#16905=DIRECTION('',(0.,0.,1.));
#16906=DIRECTION('center_axis',(0.,0.,-1.));
#16907=DIRECTION('ref_axis',(1.,0.,0.));
#16908=DIRECTION('center_axis',(0.,0.,1.));
#16909=DIRECTION('ref_axis',(1.,0.,0.));
#16910=DIRECTION('center_axis',(0.,0.,1.));
#16911=DIRECTION('ref_axis',(1.,0.,0.));
#16912=DIRECTION('',(0.,0.,1.));
#16913=DIRECTION('center_axis',(0.,0.,-1.));
#16914=DIRECTION('ref_axis',(1.,0.,0.));
#16915=DIRECTION('center_axis',(0.,0.,1.));
#16916=DIRECTION('ref_axis',(1.,0.,0.));
#16917=DIRECTION('',(0.,-1.,0.));
#16918=DIRECTION('',(-1.,0.,0.));
#16919=DIRECTION('',(0.,-1.,0.));
#16920=DIRECTION('',(1.,0.,0.));
#16921=DIRECTION('center_axis',(0.,0.,1.));
#16922=DIRECTION('ref_axis',(1.,0.,0.));
#16923=DIRECTION('',(0.,1.,0.));
#16924=DIRECTION('',(1.,0.,0.));
#16925=DIRECTION('',(0.,1.,0.));
#16926=DIRECTION('',(-1.,0.,0.));
#16927=DIRECTION('center_axis',(1.,0.,0.));
#16928=DIRECTION('ref_axis',(0.,1.,0.));
#16929=DIRECTION('',(0.,1.,0.));
#16930=DIRECTION('',(0.,0.,1.));
#16931=DIRECTION('',(0.,0.,1.));
#16932=DIRECTION('center_axis',(-1.,0.,0.));
#16933=DIRECTION('ref_axis',(0.,-1.,0.));
#16934=DIRECTION('',(0.,-1.,0.));
#16935=DIRECTION('',(0.,0.,1.));
#16936=DIRECTION('',(0.,0.,1.));
#16937=DIRECTION('center_axis',(0.,1.,0.));
#16938=DIRECTION('ref_axis',(-1.,0.,0.));
#16939=DIRECTION('',(0.,0.,1.));
#16940=DIRECTION('',(-1.,0.,0.));
#16941=DIRECTION('',(0.,0.,1.));
#16942=DIRECTION('',(-1.,0.,0.));
#16943=DIRECTION('center_axis',(-1.,0.,0.));
#16944=DIRECTION('ref_axis',(0.,-1.,0.));
#16945=DIRECTION('',(0.,0.,1.));
#16946=DIRECTION('',(0.,-1.,0.));
#16947=DIRECTION('center_axis',(1.,0.,0.));
#16948=DIRECTION('ref_axis',(0.,0.,-1.));
#16949=DIRECTION('center_axis',(1.,0.,0.));
#16950=DIRECTION('ref_axis',(0.,0.,-1.));
#16951=DIRECTION('center_axis',(1.,0.,0.));
#16952=DIRECTION('ref_axis',(0.,0.,-1.));
#16953=DIRECTION('',(1.,0.,0.));
#16954=DIRECTION('center_axis',(-1.,0.,0.));
#16955=DIRECTION('ref_axis',(0.,0.,-1.));
#16956=DIRECTION('center_axis',(1.,0.,0.));
#16957=DIRECTION('ref_axis',(0.,0.,-1.));
#16958=DIRECTION('',(1.,0.,0.));
#16959=DIRECTION('center_axis',(-1.,0.,0.));
#16960=DIRECTION('ref_axis',(0.,0.,-1.));
#16961=DIRECTION('center_axis',(1.,0.,0.));
#16962=DIRECTION('ref_axis',(0.,1.,0.));
#16963=DIRECTION('',(0.,1.,0.));
#16964=DIRECTION('',(0.,0.,1.));
#16965=DIRECTION('center_axis',(0.,-1.,0.));
#16966=DIRECTION('ref_axis',(1.,0.,0.));
#16967=DIRECTION('',(1.,0.,0.));
#16968=DIRECTION('',(1.,0.,0.));
#16969=DIRECTION('center_axis',(0.,0.,1.));
#16970=DIRECTION('ref_axis',(1.,0.,0.));
#16971=DIRECTION('center_axis',(0.,0.,1.));
#16972=DIRECTION('ref_axis',(1.,0.,0.));
#16973=DIRECTION('axis',(0.,0.,1.));
#16974=DIRECTION('refdir',(1.,0.,0.));
#16975=DIRECTION('center_axis',(1.,0.,0.));
#16976=DIRECTION('ref_axis',(0.,0.,-1.));
#16977=DIRECTION('center_axis',(1.,0.,0.));
#16978=DIRECTION('ref_axis',(0.,0.,-1.));
#16979=DIRECTION('',(1.,0.,0.));
#16980=DIRECTION('center_axis',(-1.,0.,0.));
#16981=DIRECTION('ref_axis',(0.,0.,-1.));
#16982=DIRECTION('center_axis',(1.,0.,0.));
#16983=DIRECTION('ref_axis',(0.,0.,-1.));
#16984=DIRECTION('center_axis',(1.,0.,0.));
#16985=DIRECTION('ref_axis',(0.,0.,-1.));
#16986=DIRECTION('',(1.,0.,0.));
#16987=DIRECTION('center_axis',(-1.,0.,0.));
#16988=DIRECTION('ref_axis',(0.,0.,-1.));
#16989=DIRECTION('center_axis',(1.,0.,0.));
#16990=DIRECTION('ref_axis',(0.,0.,-1.));
#16991=DIRECTION('center_axis',(1.,0.,0.));
#16992=DIRECTION('ref_axis',(0.,0.,-1.));
#16993=DIRECTION('',(1.,0.,0.));
#16994=DIRECTION('center_axis',(-1.,0.,0.));
#16995=DIRECTION('ref_axis',(0.,0.,-1.));
#16996=DIRECTION('center_axis',(1.,0.,0.));
#16997=DIRECTION('ref_axis',(0.,0.,-1.));
#16998=DIRECTION('center_axis',(1.,0.,0.));
#16999=DIRECTION('ref_axis',(0.,0.,-1.));
#17000=DIRECTION('',(1.,0.,0.));
#17001=DIRECTION('center_axis',(-1.,0.,0.));
#17002=DIRECTION('ref_axis',(0.,0.,-1.));
#17003=DIRECTION('center_axis',(1.,0.,0.));
#17004=DIRECTION('ref_axis',(0.,0.,-1.));
#17005=DIRECTION('center_axis',(1.,0.,0.));
#17006=DIRECTION('ref_axis',(0.,0.,-1.));
#17007=DIRECTION('',(-1.,0.,0.));
#17008=DIRECTION('center_axis',(-1.,0.,0.));
#17009=DIRECTION('ref_axis',(0.,0.,-1.));
#17010=DIRECTION('center_axis',(1.,0.,0.));
#17011=DIRECTION('ref_axis',(0.,0.,-1.));
#17012=DIRECTION('center_axis',(-1.,0.,0.));
#17013=DIRECTION('ref_axis',(0.,0.,-1.));
#17014=DIRECTION('center_axis',(1.,0.,0.));
#17015=DIRECTION('ref_axis',(0.,0.,-1.));
#17016=DIRECTION('',(-1.,0.,0.));
#17017=DIRECTION('center_axis',(-1.,0.,0.));
#17018=DIRECTION('ref_axis',(0.,0.,-1.));
#17019=DIRECTION('center_axis',(1.,0.,0.));
#17020=DIRECTION('ref_axis',(0.,0.,-1.));
#17021=DIRECTION('center_axis',(1.,0.,0.));
#17022=DIRECTION('ref_axis',(0.,0.,-1.));
#17023=DIRECTION('',(-1.,0.,0.));
#17024=DIRECTION('center_axis',(1.,0.,0.));
#17025=DIRECTION('ref_axis',(0.,0.,-1.));
#17026=DIRECTION('center_axis',(1.,0.,0.));
#17027=DIRECTION('ref_axis',(0.,0.,-1.));
#17028=DIRECTION('center_axis',(1.,0.,0.));
#17029=DIRECTION('ref_axis',(0.,0.,-1.));
#17030=DIRECTION('axis',(0.,0.,1.));
#17031=DIRECTION('refdir',(1.,0.,0.));
#17032=DIRECTION('center_axis',(1.,0.,0.));
#17033=DIRECTION('ref_axis',(0.,0.,-1.));
#17034=DIRECTION('center_axis',(1.,0.,0.));
#17035=DIRECTION('ref_axis',(0.,0.,-1.));
#17036=DIRECTION('',(1.,0.,0.));
#17037=DIRECTION('center_axis',(-1.,0.,0.));
#17038=DIRECTION('ref_axis',(0.,0.,-1.));
#17039=DIRECTION('center_axis',(1.,0.,0.));
#17040=DIRECTION('ref_axis',(0.,0.,-1.));
#17041=DIRECTION('center_axis',(1.,0.,0.));
#17042=DIRECTION('ref_axis',(0.,0.,-1.));
#17043=DIRECTION('',(1.,0.,0.));
#17044=DIRECTION('center_axis',(-1.,0.,0.));
#17045=DIRECTION('ref_axis',(0.,0.,-1.));
#17046=DIRECTION('center_axis',(1.,0.,0.));
#17047=DIRECTION('ref_axis',(0.,0.,-1.));
#17048=DIRECTION('center_axis',(1.,0.,0.));
#17049=DIRECTION('ref_axis',(0.,0.,-1.));
#17050=DIRECTION('',(1.,0.,0.));
#17051=DIRECTION('center_axis',(-1.,0.,0.));
#17052=DIRECTION('ref_axis',(0.,0.,-1.));
#17053=DIRECTION('center_axis',(1.,0.,0.));
#17054=DIRECTION('ref_axis',(0.,0.,-1.));
#17055=DIRECTION('center_axis',(1.,0.,0.));
#17056=DIRECTION('ref_axis',(0.,0.,-1.));
#17057=DIRECTION('',(1.,0.,0.));
#17058=DIRECTION('center_axis',(-1.,0.,0.));
#17059=DIRECTION('ref_axis',(0.,0.,-1.));
#17060=DIRECTION('center_axis',(1.,0.,0.));
#17061=DIRECTION('ref_axis',(0.,0.,-1.));
#17062=DIRECTION('center_axis',(1.,0.,0.));
#17063=DIRECTION('ref_axis',(0.,0.,-1.));
#17064=DIRECTION('',(-1.,0.,0.));
#17065=DIRECTION('center_axis',(1.,0.,0.));
#17066=DIRECTION('ref_axis',(0.,0.,-1.));
#17067=DIRECTION('center_axis',(1.,0.,0.));
#17068=DIRECTION('ref_axis',(0.,0.,-1.));
#17069=DIRECTION('center_axis',(-1.,0.,0.));
#17070=DIRECTION('ref_axis',(0.,0.,-1.));
#17071=DIRECTION('center_axis',(1.,0.,0.));
#17072=DIRECTION('ref_axis',(0.,0.,-1.));
#17073=DIRECTION('center_axis',(-1.,0.,0.));
#17074=DIRECTION('ref_axis',(0.,0.,-1.));
#17075=DIRECTION('',(-1.,0.,0.));
#17076=DIRECTION('center_axis',(1.,0.,0.));
#17077=DIRECTION('ref_axis',(0.,0.,-1.));
#17078=DIRECTION('center_axis',(1.,0.,0.));
#17079=DIRECTION('ref_axis',(0.,0.,-1.));
#17080=DIRECTION('',(-1.,0.,0.));
#17081=DIRECTION('center_axis',(1.,0.,0.));
#17082=DIRECTION('ref_axis',(0.,0.,-1.));
#17083=DIRECTION('center_axis',(1.,0.,0.));
#17084=DIRECTION('ref_axis',(0.,0.,-1.));
#17085=DIRECTION('center_axis',(1.,0.,0.));
#17086=DIRECTION('ref_axis',(0.,0.,-1.));
#17087=DIRECTION('axis',(0.,0.,1.));
#17088=DIRECTION('refdir',(1.,0.,0.));
#17089=DIRECTION('center_axis',(1.,0.,0.));
#17090=DIRECTION('ref_axis',(0.,0.,-1.));
#17091=DIRECTION('center_axis',(1.,0.,0.));
#17092=DIRECTION('ref_axis',(0.,0.,-1.));
#17093=DIRECTION('',(-1.,0.,0.));
#17094=DIRECTION('center_axis',(1.,0.,0.));
#17095=DIRECTION('ref_axis',(0.,0.,-1.));
#17096=DIRECTION('center_axis',(1.,0.,0.));
#17097=DIRECTION('ref_axis',(0.,0.,-1.));
#17098=DIRECTION('center_axis',(1.,0.,0.));
#17099=DIRECTION('ref_axis',(0.,0.,-1.));
#17100=DIRECTION('axis',(0.,0.,1.));
#17101=DIRECTION('refdir',(1.,0.,0.));
#17102=DIRECTION('center_axis',(1.,0.,0.));
#17103=DIRECTION('ref_axis',(0.,0.,-1.));
#17104=DIRECTION('center_axis',(1.,0.,0.));
#17105=DIRECTION('ref_axis',(0.,0.,-1.));
#17106=DIRECTION('',(-1.,0.,0.));
#17107=DIRECTION('center_axis',(1.,0.,0.));
#17108=DIRECTION('ref_axis',(0.,0.,-1.));
#17109=DIRECTION('center_axis',(1.,0.,0.));
#17110=DIRECTION('ref_axis',(0.,0.,-1.));
#17111=DIRECTION('center_axis',(1.,0.,0.));
#17112=DIRECTION('ref_axis',(0.,0.,-1.));
#17113=DIRECTION('axis',(0.,0.,1.));
#17114=DIRECTION('refdir',(1.,0.,0.));
#17115=DIRECTION('center_axis',(0.,1.,0.));
#17116=DIRECTION('ref_axis',(1.,0.,0.));
#17117=DIRECTION('center_axis',(0.,1.,0.));
#17118=DIRECTION('ref_axis',(1.,0.,0.));
#17119=DIRECTION('',(0.,1.,0.));
#17120=DIRECTION('center_axis',(0.,-1.,0.));
#17121=DIRECTION('ref_axis',(1.,0.,0.));
#17122=DIRECTION('center_axis',(0.,1.,0.));
#17123=DIRECTION('ref_axis',(1.,0.,0.));
#17124=DIRECTION('center_axis',(0.,1.,0.));
#17125=DIRECTION('ref_axis',(1.,0.,0.));
#17126=DIRECTION('center_axis',(0.,1.,0.));
#17127=DIRECTION('ref_axis',(1.,0.,0.));
#17128=DIRECTION('',(0.,1.,0.));
#17129=DIRECTION('center_axis',(0.,1.,0.));
#17130=DIRECTION('ref_axis',(1.,0.,0.));
#17131=DIRECTION('center_axis',(0.,1.,0.));
#17132=DIRECTION('ref_axis',(1.,0.,0.));
#17133=DIRECTION('center_axis',(0.,1.,0.));
#17134=DIRECTION('ref_axis',(1.,0.,0.));
#17135=DIRECTION('center_axis',(0.,1.,0.));
#17136=DIRECTION('ref_axis',(1.,0.,0.));
#17137=DIRECTION('',(0.,-1.,0.));
#17138=DIRECTION('center_axis',(0.,1.,0.));
#17139=DIRECTION('ref_axis',(1.,0.,0.));
#17140=DIRECTION('center_axis',(0.,1.,0.));
#17141=DIRECTION('ref_axis',(1.,0.,0.));
#17142=DIRECTION('center_axis',(0.,1.,0.));
#17143=DIRECTION('ref_axis',(1.,0.,0.));
#17144=DIRECTION('axis',(0.,0.,1.));
#17145=DIRECTION('refdir',(1.,0.,0.));
#17146=DIRECTION('center_axis',(0.,1.,0.));
#17147=DIRECTION('ref_axis',(1.,0.,0.));
#17148=DIRECTION('center_axis',(0.,-1.,0.));
#17149=DIRECTION('ref_axis',(1.,0.,0.));
#17150=DIRECTION('',(0.,-1.,0.));
#17151=DIRECTION('center_axis',(0.,-1.,0.));
#17152=DIRECTION('ref_axis',(1.,0.,0.));
#17153=DIRECTION('center_axis',(0.,1.,0.));
#17154=DIRECTION('ref_axis',(1.,0.,0.));
#17155=DIRECTION('center_axis',(0.,1.,0.));
#17156=DIRECTION('ref_axis',(1.,0.,0.));
#17157=DIRECTION('',(0.,-1.,0.));
#17158=DIRECTION('center_axis',(0.,1.,0.));
#17159=DIRECTION('ref_axis',(1.,0.,0.));
#17160=DIRECTION('center_axis',(0.,1.,0.));
#17161=DIRECTION('ref_axis',(1.,0.,0.));
#17162=DIRECTION('center_axis',(0.,1.,0.));
#17163=DIRECTION('ref_axis',(1.,0.,0.));
#17164=DIRECTION('axis',(0.,0.,1.));
#17165=DIRECTION('refdir',(1.,0.,0.));
#17166=DIRECTION('center_axis',(0.,1.,0.));
#17167=DIRECTION('ref_axis',(1.,0.,0.));
#17168=DIRECTION('center_axis',(0.,-1.,0.));
#17169=DIRECTION('ref_axis',(1.,0.,0.));
#17170=DIRECTION('',(0.,-1.,0.));
#17171=DIRECTION('center_axis',(0.,-1.,0.));
#17172=DIRECTION('ref_axis',(1.,0.,0.));
#17173=DIRECTION('center_axis',(0.,1.,0.));
#17174=DIRECTION('ref_axis',(1.,0.,0.));
#17175=DIRECTION('center_axis',(0.,1.,0.));
#17176=DIRECTION('ref_axis',(1.,0.,0.));
#17177=DIRECTION('',(0.,-1.,0.));
#17178=DIRECTION('center_axis',(0.,1.,0.));
#17179=DIRECTION('ref_axis',(1.,0.,0.));
#17180=DIRECTION('center_axis',(0.,1.,0.));
#17181=DIRECTION('ref_axis',(1.,0.,0.));
#17182=DIRECTION('center_axis',(0.,1.,0.));
#17183=DIRECTION('ref_axis',(1.,0.,0.));
#17184=DIRECTION('axis',(0.,0.,1.));
#17185=DIRECTION('refdir',(1.,0.,0.));
#17186=DIRECTION('center_axis',(0.,1.,0.));
#17187=DIRECTION('ref_axis',(1.,0.,0.));
#17188=DIRECTION('center_axis',(0.,-1.,0.));
#17189=DIRECTION('ref_axis',(1.,0.,0.));
#17190=DIRECTION('',(0.,-1.,0.));
#17191=DIRECTION('center_axis',(0.,-1.,0.));
#17192=DIRECTION('ref_axis',(1.,0.,0.));
#17193=DIRECTION('center_axis',(0.,1.,0.));
#17194=DIRECTION('ref_axis',(1.,0.,0.));
#17195=DIRECTION('center_axis',(0.,1.,0.));
#17196=DIRECTION('ref_axis',(1.,0.,0.));
#17197=DIRECTION('',(0.,-1.,0.));
#17198=DIRECTION('center_axis',(0.,1.,0.));
#17199=DIRECTION('ref_axis',(1.,0.,0.));
#17200=DIRECTION('center_axis',(0.,1.,0.));
#17201=DIRECTION('ref_axis',(1.,0.,0.));
#17202=DIRECTION('center_axis',(0.,1.,0.));
#17203=DIRECTION('ref_axis',(1.,0.,0.));
#17204=DIRECTION('axis',(0.,0.,1.));
#17205=DIRECTION('refdir',(1.,0.,0.));
#17206=DIRECTION('center_axis',(0.,1.,0.));
#17207=DIRECTION('ref_axis',(1.,0.,0.));
#17208=DIRECTION('center_axis',(0.,-1.,0.));
#17209=DIRECTION('ref_axis',(1.,0.,0.));
#17210=DIRECTION('',(0.,-1.,0.));
#17211=DIRECTION('center_axis',(0.,-1.,0.));
#17212=DIRECTION('ref_axis',(1.,0.,0.));
#17213=DIRECTION('center_axis',(0.,1.,0.));
#17214=DIRECTION('ref_axis',(1.,0.,0.));
#17215=DIRECTION('center_axis',(0.,1.,0.));
#17216=DIRECTION('ref_axis',(1.,0.,0.));
#17217=DIRECTION('',(0.,-1.,0.));
#17218=DIRECTION('center_axis',(0.,1.,0.));
#17219=DIRECTION('ref_axis',(1.,0.,0.));
#17220=DIRECTION('center_axis',(0.,1.,0.));
#17221=DIRECTION('ref_axis',(1.,0.,0.));
#17222=DIRECTION('center_axis',(0.,1.,0.));
#17223=DIRECTION('ref_axis',(1.,0.,0.));
#17224=DIRECTION('axis',(0.,0.,1.));
#17225=DIRECTION('refdir',(1.,0.,0.));
#17226=DIRECTION('center_axis',(0.,1.,0.));
#17227=DIRECTION('ref_axis',(1.,0.,0.));
#17228=DIRECTION('center_axis',(0.,-1.,0.));
#17229=DIRECTION('ref_axis',(1.,0.,0.));
#17230=DIRECTION('',(0.,-1.,0.));
#17231=DIRECTION('center_axis',(0.,-1.,0.));
#17232=DIRECTION('ref_axis',(1.,0.,0.));
#17233=DIRECTION('center_axis',(0.,1.,0.));
#17234=DIRECTION('ref_axis',(1.,0.,0.));
#17235=DIRECTION('center_axis',(0.,1.,0.));
#17236=DIRECTION('ref_axis',(1.,0.,0.));
#17237=DIRECTION('',(0.,-1.,0.));
#17238=DIRECTION('center_axis',(0.,1.,0.));
#17239=DIRECTION('ref_axis',(1.,0.,0.));
#17240=DIRECTION('center_axis',(0.,1.,0.));
#17241=DIRECTION('ref_axis',(1.,0.,0.));
#17242=DIRECTION('center_axis',(0.,1.,0.));
#17243=DIRECTION('ref_axis',(1.,0.,0.));
#17244=DIRECTION('axis',(0.,0.,1.));
#17245=DIRECTION('refdir',(1.,0.,0.));
#17246=DIRECTION('center_axis',(0.866025403784439,0.,-0.5));
#17247=DIRECTION('ref_axis',(0.5,0.,0.866025403784439));
#17248=DIRECTION('',(-0.5,0.,-0.866025403784439));
#17249=DIRECTION('',(0.,-1.,0.));
#17250=DIRECTION('',(0.5,0.,0.866025403784439));
#17251=DIRECTION('',(0.,-1.,0.));
#17252=DIRECTION('center_axis',(1.60246890531964E-16,0.,-1.));
#17253=DIRECTION('ref_axis',(1.,0.,1.60246890531964E-16));
#17254=DIRECTION('',(-1.,0.,-1.60246890531964E-16));
#17255=DIRECTION('',(0.,-1.,0.));
#17256=DIRECTION('',(1.,0.,1.60246890531964E-16));
#17257=DIRECTION('center_axis',(-0.866025403784439,0.,-0.5));
#17258=DIRECTION('ref_axis',(0.5,0.,-0.866025403784439));
#17259=DIRECTION('',(-0.5,0.,0.866025403784439));
#17260=DIRECTION('',(0.,-1.,0.));
#17261=DIRECTION('',(0.5,0.,-0.866025403784439));
#17262=DIRECTION('center_axis',(-0.866025403784439,0.,0.5));
#17263=DIRECTION('ref_axis',(-0.5,0.,-0.866025403784439));
#17264=DIRECTION('',(0.5,0.,0.866025403784439));
#17265=DIRECTION('',(0.,-1.,0.));
#17266=DIRECTION('',(-0.5,0.,-0.866025403784439));
#17267=DIRECTION('center_axis',(-1.60246890531964E-16,0.,1.));
#17268=DIRECTION('ref_axis',(-1.,0.,-1.60246890531964E-16));
#17269=DIRECTION('',(1.,0.,1.60246890531964E-16));
#17270=DIRECTION('',(0.,-1.,0.));
#17271=DIRECTION('',(-1.,0.,-1.60246890531964E-16));
#17272=DIRECTION('center_axis',(0.866025403784439,0.,0.5));
#17273=DIRECTION('ref_axis',(-0.5,0.,0.866025403784439));
#17274=DIRECTION('',(0.5,0.,-0.866025403784439));
#17275=DIRECTION('',(-0.5,0.,0.866025403784439));
#17276=DIRECTION('center_axis',(0.,1.,0.));
#17277=DIRECTION('ref_axis',(1.,0.,0.));
#17278=DIRECTION('center_axis',(0.,-1.,0.));
#17279=DIRECTION('ref_axis',(0.,0.,-1.));
#17280=DIRECTION('center_axis',(0.,1.,0.));
#17281=DIRECTION('ref_axis',(1.,0.,0.));
#17282=DIRECTION('center_axis',(0.,1.,0.));
#17283=DIRECTION('ref_axis',(1.,0.,0.));
#17284=DIRECTION('center_axis',(0.,1.,0.));
#17285=DIRECTION('ref_axis',(0.,0.,1.));
#17286=DIRECTION('center_axis',(0.,-1.,0.));
#17287=DIRECTION('ref_axis',(1.,0.,0.));
#17288=DIRECTION('center_axis',(0.,-1.,0.));
#17289=DIRECTION('ref_axis',(1.,0.,0.));
#17290=DIRECTION('center_axis',(0.,-1.,0.));
#17291=DIRECTION('ref_axis',(1.,0.,0.));
#17292=DIRECTION('',(0.707106781186547,0.707106781186548,8.65956056235493E-17));
#17293=DIRECTION('center_axis',(0.,-1.,0.));
#17294=DIRECTION('ref_axis',(1.,0.,0.));
#17295=DIRECTION('center_axis',(0.,-1.,0.));
#17296=DIRECTION('ref_axis',(1.,0.,0.));
#17297=DIRECTION('',(0.,1.,0.));
#17298=DIRECTION('center_axis',(0.,1.,0.));
#17299=DIRECTION('ref_axis',(1.,0.,0.));
#17300=DIRECTION('center_axis',(0.,-1.,0.));
#17301=DIRECTION('ref_axis',(1.,0.,0.));
#17302=DIRECTION('',(-0.707106781186547,0.707106781186548,-8.65956056235493E-17));
#17303=DIRECTION('center_axis',(0.,-1.,0.));
#17304=DIRECTION('ref_axis',(0.,0.,-1.));
#17305=DIRECTION('center_axis',(0.,-1.,0.));
#17306=DIRECTION('ref_axis',(1.,0.,0.));
#17307=DIRECTION('center_axis',(0.,1.,0.));
#17308=DIRECTION('ref_axis',(1.,0.,0.));
#17309=DIRECTION('center_axis',(0.,1.,0.));
#17310=DIRECTION('ref_axis',(1.,0.,0.));
#17311=DIRECTION('',(-0.447213595499958,0.894427190999916,-5.47678698264203E-17));
#17312=DIRECTION('center_axis',(0.,-1.,0.));
#17313=DIRECTION('ref_axis',(1.,0.,0.));
#17314=DIRECTION('',(0.,1.,0.));
#17315=DIRECTION('axis',(0.,0.,1.));
#17316=DIRECTION('refdir',(1.,0.,0.));
#17317=DIRECTION('axis',(0.,0.,1.));
#17318=DIRECTION('refdir',(1.,0.,0.));
#17319=DIRECTION('center_axis',(0.,0.,1.));
#17320=DIRECTION('ref_axis',(1.,0.,0.));
#17321=DIRECTION('center_axis',(0.,0.,1.));
#17322=DIRECTION('ref_axis',(1.,0.,0.));
#17323=DIRECTION('',(0.,0.,1.));
#17324=DIRECTION('center_axis',(0.,0.,-1.));
#17325=DIRECTION('ref_axis',(1.,0.,0.));
#17326=DIRECTION('center_axis',(0.,0.,1.));
#17327=DIRECTION('ref_axis',(1.,0.,0.));
#17328=DIRECTION('center_axis',(0.,0.,1.));
#17329=DIRECTION('ref_axis',(1.,0.,0.));
#17330=DIRECTION('',(0.,0.,1.));
#17331=DIRECTION('center_axis',(0.,0.,-1.));
#17332=DIRECTION('ref_axis',(1.,0.,0.));
#17333=DIRECTION('center_axis',(0.,0.,1.));
#17334=DIRECTION('ref_axis',(1.,0.,0.));
#17335=DIRECTION('center_axis',(0.,0.,1.));
#17336=DIRECTION('ref_axis',(1.,0.,0.));
#17337=DIRECTION('',(0.,0.,1.));
#17338=DIRECTION('center_axis',(0.,0.,-1.));
#17339=DIRECTION('ref_axis',(1.,0.,0.));
#17340=DIRECTION('center_axis',(0.,0.,1.));
#17341=DIRECTION('ref_axis',(1.,0.,0.));
#17342=DIRECTION('center_axis',(0.,0.,1.));
#17343=DIRECTION('ref_axis',(1.,0.,0.));
#17344=DIRECTION('',(0.,0.,1.));
#17345=DIRECTION('center_axis',(0.,0.,-1.));
#17346=DIRECTION('ref_axis',(1.,0.,0.));
#17347=DIRECTION('center_axis',(0.,0.,1.));
#17348=DIRECTION('ref_axis',(1.,0.,0.));
#17349=DIRECTION('center_axis',(0.,0.,1.));
#17350=DIRECTION('ref_axis',(1.,0.,0.));
#17351=DIRECTION('',(0.,0.,1.));
#17352=DIRECTION('center_axis',(0.,0.,-1.));
#17353=DIRECTION('ref_axis',(1.,0.,0.));
#17354=DIRECTION('center_axis',(0.,0.,1.));
#17355=DIRECTION('ref_axis',(1.,0.,0.));
#17356=DIRECTION('center_axis',(0.,0.,1.));
#17357=DIRECTION('ref_axis',(1.,0.,0.));
#17358=DIRECTION('',(0.,0.,1.));
#17359=DIRECTION('center_axis',(0.,0.,-1.));
#17360=DIRECTION('ref_axis',(1.,0.,0.));
#17361=DIRECTION('center_axis',(0.,0.,1.));
#17362=DIRECTION('ref_axis',(1.,0.,0.));
#17363=DIRECTION('center_axis',(0.,0.,1.));
#17364=DIRECTION('ref_axis',(1.,0.,0.));
#17365=DIRECTION('',(0.,0.,1.));
#17366=DIRECTION('center_axis',(0.,0.,-1.));
#17367=DIRECTION('ref_axis',(1.,0.,0.));
#17368=DIRECTION('center_axis',(0.,0.,1.));
#17369=DIRECTION('ref_axis',(1.,0.,0.));
#17370=DIRECTION('center_axis',(0.,0.,1.));
#17371=DIRECTION('ref_axis',(1.,0.,0.));
#17372=DIRECTION('',(0.,0.,1.));
#17373=DIRECTION('center_axis',(0.,0.,-1.));
#17374=DIRECTION('ref_axis',(1.,0.,0.));
#17375=DIRECTION('center_axis',(0.,1.,0.));
#17376=DIRECTION('ref_axis',(-1.,0.,0.));
#17377=DIRECTION('',(-1.,0.,0.));
#17378=DIRECTION('',(0.,0.,1.));
#17379=DIRECTION('',(-1.,0.,0.));
#17380=DIRECTION('',(0.,0.,1.));
#17381=DIRECTION('center_axis',(1.,0.,0.));
#17382=DIRECTION('ref_axis',(0.,1.,0.));
#17383=DIRECTION('',(0.,1.,0.));
#17384=DIRECTION('',(0.,1.,0.));
#17385=DIRECTION('',(0.,0.,1.));
#17386=DIRECTION('center_axis',(0.,-1.,0.));
#17387=DIRECTION('ref_axis',(1.,0.,0.));
#17388=DIRECTION('',(1.,0.,0.));
#17389=DIRECTION('',(1.,0.,0.));
#17390=DIRECTION('',(0.,0.,1.));
#17391=DIRECTION('center_axis',(-1.,0.,0.));
#17392=DIRECTION('ref_axis',(0.,-1.,0.));
#17393=DIRECTION('',(0.,-1.,0.));
#17394=DIRECTION('',(0.,-1.,0.));
#17395=DIRECTION('center_axis',(0.,0.,1.));
#17396=DIRECTION('ref_axis',(1.,0.,0.));
#17397=DIRECTION('center_axis',(0.,0.,1.));
#17398=DIRECTION('ref_axis',(1.,0.,0.));
#17399=DIRECTION('axis',(0.,0.,1.));
#17400=DIRECTION('refdir',(1.,0.,0.));
#17401=DIRECTION('center_axis',(0.,0.,1.));
#17402=DIRECTION('ref_axis',(1.,0.,0.));
#17403=DIRECTION('center_axis',(0.,0.,1.));
#17404=DIRECTION('ref_axis',(1.,0.,0.));
#17405=DIRECTION('',(0.,0.,1.));
#17406=DIRECTION('center_axis',(0.,0.,-1.));
#17407=DIRECTION('ref_axis',(1.,0.,0.));
#17408=DIRECTION('center_axis',(0.,0.,1.));
#17409=DIRECTION('ref_axis',(1.,0.,0.));
#17410=DIRECTION('center_axis',(0.,0.,1.));
#17411=DIRECTION('ref_axis',(1.,0.,0.));
#17412=DIRECTION('',(0.,0.,1.));
#17413=DIRECTION('center_axis',(0.,0.,-1.));
#17414=DIRECTION('ref_axis',(1.,0.,0.));
#17415=DIRECTION('center_axis',(0.,0.,1.));
#17416=DIRECTION('ref_axis',(1.,0.,0.));
#17417=DIRECTION('center_axis',(0.,0.,1.));
#17418=DIRECTION('ref_axis',(1.,0.,0.));
#17419=DIRECTION('',(0.,0.,1.));
#17420=DIRECTION('center_axis',(0.,0.,-1.));
#17421=DIRECTION('ref_axis',(1.,0.,0.));
#17422=DIRECTION('center_axis',(0.,0.,1.));
#17423=DIRECTION('ref_axis',(1.,0.,0.));
#17424=DIRECTION('center_axis',(0.,0.,1.));
#17425=DIRECTION('ref_axis',(1.,0.,0.));
#17426=DIRECTION('',(0.,0.,1.));
#17427=DIRECTION('center_axis',(0.,0.,-1.));
#17428=DIRECTION('ref_axis',(1.,0.,0.));
#17429=DIRECTION('center_axis',(0.,0.,1.));
#17430=DIRECTION('ref_axis',(1.,0.,0.));
#17431=DIRECTION('',(0.,-1.,0.));
#17432=DIRECTION('',(-1.,0.,0.));
#17433=DIRECTION('',(0.,1.,0.));
#17434=DIRECTION('',(1.,0.,0.));
#17435=DIRECTION('',(1.,0.,0.));
#17436=DIRECTION('',(0.,1.,0.));
#17437=DIRECTION('',(-1.,0.,0.));
#17438=DIRECTION('',(0.,-1.,0.));
#17439=DIRECTION('center_axis',(0.,1.,0.));
#17440=DIRECTION('ref_axis',(-1.,0.,0.));
#17441=DIRECTION('',(0.,0.,1.));
#17442=DIRECTION('',(-1.,0.,0.));
#17443=DIRECTION('',(0.,0.,1.));
#17444=DIRECTION('center_axis',(1.,0.,0.));
#17445=DIRECTION('ref_axis',(0.,1.,0.));
#17446=DIRECTION('',(0.,1.,0.));
#17447=DIRECTION('',(0.,0.,1.));
#17448=DIRECTION('center_axis',(0.,-1.,0.));
#17449=DIRECTION('ref_axis',(1.,0.,0.));
#17450=DIRECTION('',(1.,0.,0.));
#17451=DIRECTION('',(0.,0.,1.));
#17452=DIRECTION('center_axis',(-1.,0.,0.));
#17453=DIRECTION('ref_axis',(0.,-1.,0.));
#17454=DIRECTION('',(0.,-1.,0.));
#17455=DIRECTION('center_axis',(0.,-1.,0.));
#17456=DIRECTION('ref_axis',(1.,0.,0.));
#17457=DIRECTION('',(0.,0.,1.));
#17458=DIRECTION('',(1.,0.,0.));
#17459=DIRECTION('',(0.,0.,1.));
#17460=DIRECTION('center_axis',(0.,1.,0.));
#17461=DIRECTION('ref_axis',(1.,0.,0.));
#17462=DIRECTION('center_axis',(-1.,0.,0.));
#17463=DIRECTION('ref_axis',(0.,-1.,0.));
#17464=DIRECTION('',(0.,0.,1.));
#17465=DIRECTION('',(0.,-1.,0.));
#17466=DIRECTION('center_axis',(1.,0.,0.));
#17467=DIRECTION('ref_axis',(0.,0.,-1.));
#17468=DIRECTION('center_axis',(1.,0.,0.));
#17469=DIRECTION('ref_axis',(0.,0.,-1.));
#17470=DIRECTION('center_axis',(0.,1.,0.));
#17471=DIRECTION('ref_axis',(1.,0.,0.));
#17472=DIRECTION('',(0.,1.,0.));
#17473=DIRECTION('center_axis',(0.,-1.,0.));
#17474=DIRECTION('ref_axis',(1.,0.,0.));
#17475=DIRECTION('center_axis',(1.,0.,0.));
#17476=DIRECTION('ref_axis',(0.,0.,-1.));
#17477=DIRECTION('',(1.,0.,0.));
#17478=DIRECTION('center_axis',(-1.,0.,0.));
#17479=DIRECTION('ref_axis',(0.,0.,-1.));
#17480=DIRECTION('center_axis',(1.,0.,0.));
#17481=DIRECTION('ref_axis',(0.,0.,-1.));
#17482=DIRECTION('',(1.,0.,0.));
#17483=DIRECTION('center_axis',(-1.,0.,0.));
#17484=DIRECTION('ref_axis',(0.,0.,-1.));
#17485=DIRECTION('center_axis',(0.,1.,0.));
#17486=DIRECTION('ref_axis',(-1.,0.,0.));
#17487=DIRECTION('',(0.,0.,1.));
#17488=DIRECTION('',(-1.,0.,0.));
#17489=DIRECTION('center_axis',(1.,0.,0.));
#17490=DIRECTION('ref_axis',(0.,1.,0.));
#17491=DIRECTION('',(0.,1.,0.));
#17492=DIRECTION('center_axis',(0.,0.,1.));
#17493=DIRECTION('ref_axis',(1.,0.,0.));
#17494=DIRECTION('center_axis',(0.,0.,1.));
#17495=DIRECTION('ref_axis',(1.,0.,0.));
#17496=DIRECTION('axis',(0.,0.,1.));
#17497=DIRECTION('refdir',(1.,0.,0.));
#17498=DIRECTION('center_axis',(0.,0.,1.));
#17499=DIRECTION('ref_axis',(1.,0.,0.));
#17500=DIRECTION('center_axis',(0.,0.,1.));
#17501=DIRECTION('ref_axis',(1.,0.,0.));
#17502=DIRECTION('',(0.,0.,1.));
#17503=DIRECTION('center_axis',(0.,0.,-1.));
#17504=DIRECTION('ref_axis',(1.,0.,0.));
#17505=DIRECTION('center_axis',(0.,0.,1.));
#17506=DIRECTION('ref_axis',(1.,0.,0.));
#17507=DIRECTION('center_axis',(0.,0.,1.));
#17508=DIRECTION('ref_axis',(1.,0.,0.));
#17509=DIRECTION('',(0.,0.,1.));
#17510=DIRECTION('center_axis',(0.,0.,-1.));
#17511=DIRECTION('ref_axis',(1.,0.,0.));
#17512=DIRECTION('center_axis',(0.,0.,1.));
#17513=DIRECTION('ref_axis',(1.,0.,0.));
#17514=DIRECTION('center_axis',(0.,0.,1.));
#17515=DIRECTION('ref_axis',(1.,0.,0.));
#17516=DIRECTION('',(0.,0.,1.));
#17517=DIRECTION('center_axis',(0.,0.,-1.));
#17518=DIRECTION('ref_axis',(1.,0.,0.));
#17519=DIRECTION('center_axis',(0.,0.,1.));
#17520=DIRECTION('ref_axis',(1.,0.,0.));
#17521=DIRECTION('center_axis',(0.,0.,1.));
#17522=DIRECTION('ref_axis',(1.,0.,0.));
#17523=DIRECTION('',(0.,0.,1.));
#17524=DIRECTION('center_axis',(0.,0.,-1.));
#17525=DIRECTION('ref_axis',(1.,0.,0.));
#17526=DIRECTION('center_axis',(0.,0.,1.));
#17527=DIRECTION('ref_axis',(1.,0.,0.));
#17528=DIRECTION('',(0.,1.,0.));
#17529=DIRECTION('',(1.,0.,0.));
#17530=DIRECTION('',(0.,-1.,0.));
#17531=DIRECTION('',(-1.,0.,0.));
#17532=DIRECTION('center_axis',(1.,0.,0.));
#17533=DIRECTION('ref_axis',(0.,1.,0.));
#17534=DIRECTION('',(0.,1.,0.));
#17535=DIRECTION('',(0.,0.,1.));
#17536=DIRECTION('',(0.,1.,0.));
#17537=DIRECTION('',(0.,0.,1.));
#17538=DIRECTION('center_axis',(-1.,0.,0.));
#17539=DIRECTION('ref_axis',(0.,-1.,0.));
#17540=DIRECTION('',(0.,0.,1.));
#17541=DIRECTION('',(0.,-1.,0.));
#17542=DIRECTION('',(0.,0.,1.));
#17543=DIRECTION('center_axis',(0.,0.,1.));
#17544=DIRECTION('ref_axis',(1.,0.,0.));
#17545=DIRECTION('',(0.,-1.,0.));
#17546=DIRECTION('',(-1.,0.,0.));
#17547=DIRECTION('',(1.,0.,0.));
#17548=DIRECTION('center_axis',(1.,0.,0.));
#17549=DIRECTION('ref_axis',(0.,1.,0.));
#17550=DIRECTION('',(0.,0.,1.));
#17551=DIRECTION('',(0.,1.,0.));
#17552=DIRECTION('',(0.,0.,1.));
#17553=DIRECTION('center_axis',(-1.,0.,0.));
#17554=DIRECTION('ref_axis',(0.,0.,-1.));
#17555=DIRECTION('center_axis',(-1.,0.,0.));
#17556=DIRECTION('ref_axis',(0.,0.,-1.));
#17557=DIRECTION('center_axis',(0.,-1.,0.));
#17558=DIRECTION('ref_axis',(1.,0.,0.));
#17559=DIRECTION('',(0.,0.,1.));
#17560=DIRECTION('',(1.,0.,0.));
#17561=DIRECTION('',(1.,0.,0.));
#17562=DIRECTION('center_axis',(1.,0.,0.));
#17563=DIRECTION('ref_axis',(0.,0.,-1.));
#17564=DIRECTION('center_axis',(1.,0.,0.));
#17565=DIRECTION('ref_axis',(0.,0.,-1.));
#17566=DIRECTION('',(1.,0.,0.));
#17567=DIRECTION('center_axis',(1.,0.,0.));
#17568=DIRECTION('ref_axis',(0.,0.,-1.));
#17569=DIRECTION('center_axis',(1.,0.,0.));
#17570=DIRECTION('ref_axis',(0.,0.,-1.));
#17571=DIRECTION('',(1.,0.,0.));
#17572=DIRECTION('center_axis',(0.,1.,0.));
#17573=DIRECTION('ref_axis',(-1.,0.,0.));
#17574=DIRECTION('',(-1.,0.,0.));
#17575=DIRECTION('',(0.,0.,1.));
#17576=DIRECTION('',(-1.,0.,0.));
#17577=DIRECTION('center_axis',(-1.,0.,0.));
#17578=DIRECTION('ref_axis',(0.,-1.,0.));
#17579=DIRECTION('',(0.,-1.,0.));
#17580=DIRECTION('center_axis',(0.,0.,1.));
#17581=DIRECTION('ref_axis',(1.,0.,0.));
#17582=DIRECTION('center_axis',(0.,0.,1.));
#17583=DIRECTION('ref_axis',(1.,0.,0.));
#17584=DIRECTION('axis',(0.,0.,1.));
#17585=DIRECTION('refdir',(1.,0.,0.));
#17586=DIRECTION('center_axis',(1.,0.,0.));
#17587=DIRECTION('ref_axis',(0.,0.,-1.));
#17588=DIRECTION('center_axis',(1.,0.,0.));
#17589=DIRECTION('ref_axis',(0.,0.,-1.));
#17590=DIRECTION('',(-1.,0.,0.));
#17591=DIRECTION('center_axis',(1.,0.,0.));
#17592=DIRECTION('ref_axis',(0.,0.,-1.));
#17593=DIRECTION('center_axis',(1.,0.,0.));
#17594=DIRECTION('ref_axis',(0.,0.,-1.));
#17595=DIRECTION('center_axis',(1.,0.,0.));
#17596=DIRECTION('ref_axis',(0.,0.,-1.));
#17597=DIRECTION('axis',(0.,0.,1.));
#17598=DIRECTION('refdir',(1.,0.,0.));
#17599=DIRECTION('center_axis',(1.,0.,0.));
#17600=DIRECTION('ref_axis',(0.,0.,-1.));
#17601=DIRECTION('center_axis',(1.,0.,0.));
#17602=DIRECTION('ref_axis',(0.,0.,-1.));
#17603=DIRECTION('',(-1.,0.,0.));
#17604=DIRECTION('center_axis',(1.,0.,0.));
#17605=DIRECTION('ref_axis',(0.,0.,-1.));
#17606=DIRECTION('center_axis',(1.,0.,0.));
#17607=DIRECTION('ref_axis',(0.,0.,-1.));
#17608=DIRECTION('center_axis',(1.,0.,0.));
#17609=DIRECTION('ref_axis',(0.,0.,-1.));
#17610=DIRECTION('axis',(0.,0.,1.));
#17611=DIRECTION('refdir',(1.,0.,0.));
#17612=DIRECTION('center_axis',(0.,1.,0.));
#17613=DIRECTION('ref_axis',(1.,0.,0.));
#17614=DIRECTION('center_axis',(0.,1.,0.));
#17615=DIRECTION('ref_axis',(1.,0.,0.));
#17616=DIRECTION('',(0.,1.,0.));
#17617=DIRECTION('center_axis',(0.,-1.,0.));
#17618=DIRECTION('ref_axis',(1.,0.,0.));
#17619=DIRECTION('center_axis',(0.,1.,0.));
#17620=DIRECTION('ref_axis',(1.,0.,0.));
#17621=DIRECTION('center_axis',(0.,1.,0.));
#17622=DIRECTION('ref_axis',(1.,0.,0.));
#17623=DIRECTION('center_axis',(0.,1.,0.));
#17624=DIRECTION('ref_axis',(1.,0.,0.));
#17625=DIRECTION('',(0.,1.,0.));
#17626=DIRECTION('center_axis',(0.,1.,0.));
#17627=DIRECTION('ref_axis',(1.,0.,0.));
#17628=DIRECTION('center_axis',(0.,1.,0.));
#17629=DIRECTION('ref_axis',(1.,0.,0.));
#17630=DIRECTION('center_axis',(0.,1.,0.));
#17631=DIRECTION('ref_axis',(1.,0.,0.));
#17632=DIRECTION('center_axis',(0.,1.,0.));
#17633=DIRECTION('ref_axis',(1.,0.,0.));
#17634=DIRECTION('',(0.,-1.,0.));
#17635=DIRECTION('center_axis',(0.,1.,0.));
#17636=DIRECTION('ref_axis',(1.,0.,0.));
#17637=DIRECTION('center_axis',(0.,1.,0.));
#17638=DIRECTION('ref_axis',(1.,0.,0.));
#17639=DIRECTION('center_axis',(0.,1.,0.));
#17640=DIRECTION('ref_axis',(1.,0.,0.));
#17641=DIRECTION('axis',(0.,0.,1.));
#17642=DIRECTION('refdir',(1.,0.,0.));
#17643=DIRECTION('center_axis',(0.,1.,0.));
#17644=DIRECTION('ref_axis',(1.,0.,0.));
#17645=DIRECTION('center_axis',(0.,-1.,0.));
#17646=DIRECTION('ref_axis',(1.,0.,0.));
#17647=DIRECTION('',(0.,-1.,0.));
#17648=DIRECTION('center_axis',(0.,-1.,0.));
#17649=DIRECTION('ref_axis',(1.,0.,0.));
#17650=DIRECTION('center_axis',(0.,1.,0.));
#17651=DIRECTION('ref_axis',(1.,0.,0.));
#17652=DIRECTION('center_axis',(0.,1.,0.));
#17653=DIRECTION('ref_axis',(1.,0.,0.));
#17654=DIRECTION('',(0.,-1.,0.));
#17655=DIRECTION('center_axis',(0.,1.,0.));
#17656=DIRECTION('ref_axis',(1.,0.,0.));
#17657=DIRECTION('center_axis',(0.,1.,0.));
#17658=DIRECTION('ref_axis',(1.,0.,0.));
#17659=DIRECTION('center_axis',(0.,1.,0.));
#17660=DIRECTION('ref_axis',(1.,0.,0.));
#17661=DIRECTION('axis',(0.,0.,1.));
#17662=DIRECTION('refdir',(1.,0.,0.));
#17663=DIRECTION('center_axis',(0.,1.,0.));
#17664=DIRECTION('ref_axis',(1.,0.,0.));
#17665=DIRECTION('center_axis',(0.,-1.,0.));
#17666=DIRECTION('ref_axis',(1.,0.,0.));
#17667=DIRECTION('',(0.,-1.,0.));
#17668=DIRECTION('center_axis',(0.,-1.,0.));
#17669=DIRECTION('ref_axis',(1.,0.,0.));
#17670=DIRECTION('center_axis',(0.,1.,0.));
#17671=DIRECTION('ref_axis',(1.,0.,0.));
#17672=DIRECTION('center_axis',(0.,1.,0.));
#17673=DIRECTION('ref_axis',(1.,0.,0.));
#17674=DIRECTION('',(0.,-1.,0.));
#17675=DIRECTION('center_axis',(0.,1.,0.));
#17676=DIRECTION('ref_axis',(1.,0.,0.));
#17677=DIRECTION('center_axis',(0.,1.,0.));
#17678=DIRECTION('ref_axis',(1.,0.,0.));
#17679=DIRECTION('center_axis',(0.,1.,0.));
#17680=DIRECTION('ref_axis',(1.,0.,0.));
#17681=DIRECTION('axis',(0.,0.,1.));
#17682=DIRECTION('refdir',(1.,0.,0.));
#17683=DIRECTION('center_axis',(0.,1.,0.));
#17684=DIRECTION('ref_axis',(1.,0.,0.));
#17685=DIRECTION('center_axis',(0.,-1.,0.));
#17686=DIRECTION('ref_axis',(1.,0.,0.));
#17687=DIRECTION('',(0.,-1.,0.));
#17688=DIRECTION('center_axis',(0.,-1.,0.));
#17689=DIRECTION('ref_axis',(1.,0.,0.));
#17690=DIRECTION('center_axis',(0.,1.,0.));
#17691=DIRECTION('ref_axis',(1.,0.,0.));
#17692=DIRECTION('center_axis',(0.,1.,0.));
#17693=DIRECTION('ref_axis',(1.,0.,0.));
#17694=DIRECTION('',(0.,-1.,0.));
#17695=DIRECTION('center_axis',(0.,1.,0.));
#17696=DIRECTION('ref_axis',(1.,0.,0.));
#17697=DIRECTION('center_axis',(0.,1.,0.));
#17698=DIRECTION('ref_axis',(1.,0.,0.));
#17699=DIRECTION('center_axis',(0.,1.,0.));
#17700=DIRECTION('ref_axis',(1.,0.,0.));
#17701=DIRECTION('axis',(0.,0.,1.));
#17702=DIRECTION('refdir',(1.,0.,0.));
#17703=DIRECTION('center_axis',(0.,1.,0.));
#17704=DIRECTION('ref_axis',(1.,0.,0.));
#17705=DIRECTION('center_axis',(0.,-1.,0.));
#17706=DIRECTION('ref_axis',(1.,0.,0.));
#17707=DIRECTION('',(0.,-1.,0.));
#17708=DIRECTION('center_axis',(0.,-1.,0.));
#17709=DIRECTION('ref_axis',(1.,0.,0.));
#17710=DIRECTION('center_axis',(0.,1.,0.));
#17711=DIRECTION('ref_axis',(1.,0.,0.));
#17712=DIRECTION('center_axis',(0.,1.,0.));
#17713=DIRECTION('ref_axis',(1.,0.,0.));
#17714=DIRECTION('',(0.,-1.,0.));
#17715=DIRECTION('center_axis',(0.,1.,0.));
#17716=DIRECTION('ref_axis',(1.,0.,0.));
#17717=DIRECTION('center_axis',(0.,1.,0.));
#17718=DIRECTION('ref_axis',(1.,0.,0.));
#17719=DIRECTION('center_axis',(0.,1.,0.));
#17720=DIRECTION('ref_axis',(1.,0.,0.));
#17721=DIRECTION('axis',(0.,0.,1.));
#17722=DIRECTION('refdir',(1.,0.,0.));
#17723=DIRECTION('center_axis',(0.,1.,0.));
#17724=DIRECTION('ref_axis',(1.,0.,0.));
#17725=DIRECTION('center_axis',(0.,-1.,0.));
#17726=DIRECTION('ref_axis',(1.,0.,0.));
#17727=DIRECTION('',(0.,-1.,0.));
#17728=DIRECTION('center_axis',(0.,-1.,0.));
#17729=DIRECTION('ref_axis',(1.,0.,0.));
#17730=DIRECTION('center_axis',(0.,1.,0.));
#17731=DIRECTION('ref_axis',(1.,0.,0.));
#17732=DIRECTION('center_axis',(0.,1.,0.));
#17733=DIRECTION('ref_axis',(1.,0.,0.));
#17734=DIRECTION('',(0.,-1.,0.));
#17735=DIRECTION('center_axis',(0.,1.,0.));
#17736=DIRECTION('ref_axis',(1.,0.,0.));
#17737=DIRECTION('center_axis',(0.,1.,0.));
#17738=DIRECTION('ref_axis',(1.,0.,0.));
#17739=DIRECTION('center_axis',(0.,1.,0.));
#17740=DIRECTION('ref_axis',(1.,0.,0.));
#17741=DIRECTION('axis',(0.,0.,1.));
#17742=DIRECTION('refdir',(1.,0.,0.));
#17743=DIRECTION('center_axis',(0.,1.,0.));
#17744=DIRECTION('ref_axis',(1.,0.,0.));
#17745=DIRECTION('center_axis',(0.,-1.,0.));
#17746=DIRECTION('ref_axis',(1.,0.,0.));
#17747=DIRECTION('',(0.,-1.,0.));
#17748=DIRECTION('center_axis',(0.,-1.,0.));
#17749=DIRECTION('ref_axis',(1.,0.,0.));
#17750=DIRECTION('center_axis',(0.,1.,0.));
#17751=DIRECTION('ref_axis',(1.,0.,0.));
#17752=DIRECTION('center_axis',(0.,1.,0.));
#17753=DIRECTION('ref_axis',(1.,0.,0.));
#17754=DIRECTION('',(0.,-1.,0.));
#17755=DIRECTION('center_axis',(0.,1.,0.));
#17756=DIRECTION('ref_axis',(1.,0.,0.));
#17757=DIRECTION('center_axis',(0.,1.,0.));
#17758=DIRECTION('ref_axis',(1.,0.,0.));
#17759=DIRECTION('center_axis',(0.,1.,0.));
#17760=DIRECTION('ref_axis',(1.,0.,0.));
#17761=DIRECTION('axis',(0.,0.,1.));
#17762=DIRECTION('refdir',(1.,0.,0.));
#17763=DIRECTION('center_axis',(0.,1.,0.));
#17764=DIRECTION('ref_axis',(0.,0.,1.));
#17765=DIRECTION('center_axis',(0.,-1.,0.));
#17766=DIRECTION('ref_axis',(1.,0.,0.));
#17767=DIRECTION('center_axis',(0.,-1.,0.));
#17768=DIRECTION('ref_axis',(1.,0.,0.));
#17769=DIRECTION('center_axis',(0.,-1.,0.));
#17770=DIRECTION('ref_axis',(1.,0.,0.));
#17771=DIRECTION('',(0.707106781186548,0.707106781186547,8.65956056235493E-17));
#17772=DIRECTION('center_axis',(0.,-1.,0.));
#17773=DIRECTION('ref_axis',(1.,0.,0.));
#17774=DIRECTION('center_axis',(0.,-1.,0.));
#17775=DIRECTION('ref_axis',(1.,0.,0.));
#17776=DIRECTION('',(0.,1.,0.));
#17777=DIRECTION('center_axis',(0.,1.,0.));
#17778=DIRECTION('ref_axis',(1.,0.,0.));
#17779=DIRECTION('center_axis',(0.,-1.,0.));
#17780=DIRECTION('ref_axis',(1.,0.,0.));
#17781=DIRECTION('',(-0.707106781186547,0.707106781186548,-8.65956056235493E-17));
#17782=DIRECTION('center_axis',(0.,-1.,0.));
#17783=DIRECTION('ref_axis',(0.,0.,-1.));
#17784=DIRECTION('center_axis',(0.,-1.,0.));
#17785=DIRECTION('ref_axis',(1.,0.,0.));
#17786=DIRECTION('center_axis',(0.,1.,0.));
#17787=DIRECTION('ref_axis',(1.,0.,0.));
#17788=DIRECTION('center_axis',(0.,1.,0.));
#17789=DIRECTION('ref_axis',(1.,0.,0.));
#17790=DIRECTION('',(-0.447213595499958,0.894427190999916,-5.47678698264203E-17));
#17791=DIRECTION('center_axis',(0.,-1.,0.));
#17792=DIRECTION('ref_axis',(1.,0.,0.));
#17793=DIRECTION('center_axis',(0.,1.,0.));
#17794=DIRECTION('ref_axis',(1.,0.,0.));
#17795=DIRECTION('',(0.,1.,0.));
#17796=DIRECTION('center_axis',(0.,1.,0.));
#17797=DIRECTION('ref_axis',(1.,0.,0.));
#17798=DIRECTION('center_axis',(0.,-1.,0.));
#17799=DIRECTION('ref_axis',(1.,0.,0.));
#17800=DIRECTION('',(-0.707106781186547,0.707106781186548,-8.65956056235493E-17));
#17801=DIRECTION('center_axis',(0.,-1.,0.));
#17802=DIRECTION('ref_axis',(0.,0.,-1.));
#17803=DIRECTION('center_axis',(0.866025403784439,0.,-0.5));
#17804=DIRECTION('ref_axis',(0.5,0.,0.866025403784439));
#17805=DIRECTION('',(-0.5,0.,-0.866025403784439));
#17806=DIRECTION('',(0.,-1.,0.));
#17807=DIRECTION('',(0.5,0.,0.866025403784439));
#17808=DIRECTION('',(0.,-1.,0.));
#17809=DIRECTION('center_axis',(1.20185167898973E-16,0.,-1.));
#17810=DIRECTION('ref_axis',(1.,0.,1.20185167898973E-16));
#17811=DIRECTION('',(-1.,0.,-1.20185167898973E-16));
#17812=DIRECTION('',(0.,-1.,0.));
#17813=DIRECTION('',(1.,0.,1.20185167898973E-16));
#17814=DIRECTION('center_axis',(-0.866025403784439,0.,-0.5));
#17815=DIRECTION('ref_axis',(0.5,0.,-0.866025403784439));
#17816=DIRECTION('',(-0.5,0.,0.866025403784439));
#17817=DIRECTION('',(0.,-1.,0.));
#17818=DIRECTION('',(0.5,0.,-0.866025403784439));
#17819=DIRECTION('center_axis',(-0.866025403784439,0.,0.5));
#17820=DIRECTION('ref_axis',(-0.5,0.,-0.866025403784439));
#17821=DIRECTION('',(0.5,0.,0.866025403784439));
#17822=DIRECTION('',(0.,-1.,0.));
#17823=DIRECTION('',(-0.5,0.,-0.866025403784439));
#17824=DIRECTION('center_axis',(-2.40370335797945E-16,0.,1.));
#17825=DIRECTION('ref_axis',(-1.,0.,-2.40370335797945E-16));
#17826=DIRECTION('',(1.,0.,2.40370335797945E-16));
#17827=DIRECTION('',(0.,-1.,0.));
#17828=DIRECTION('',(-1.,0.,-2.40370335797945E-16));
#17829=DIRECTION('center_axis',(0.866025403784439,0.,0.5));
#17830=DIRECTION('ref_axis',(-0.5,0.,0.866025403784439));
#17831=DIRECTION('',(0.5,0.,-0.866025403784439));
#17832=DIRECTION('',(-0.5,0.,0.866025403784439));
#17833=DIRECTION('center_axis',(0.,1.,0.));
#17834=DIRECTION('ref_axis',(1.,0.,0.));
#17835=DIRECTION('center_axis',(0.,-1.,0.));
#17836=DIRECTION('ref_axis',(0.,0.,-1.));
#17837=DIRECTION('axis',(0.,0.,1.));
#17838=DIRECTION('refdir',(1.,0.,0.));
#17839=DIRECTION('axis',(0.,0.,1.));
#17840=DIRECTION('refdir',(1.,0.,0.));
#17841=DIRECTION('center_axis',(1.,0.,0.));
#17842=DIRECTION('ref_axis',(0.,0.,-1.));
#17843=DIRECTION('center_axis',(1.,0.,0.));
#17844=DIRECTION('ref_axis',(0.,0.,-1.));
#17845=DIRECTION('',(1.,0.,0.));
#17846=DIRECTION('center_axis',(-1.,0.,0.));
#17847=DIRECTION('ref_axis',(0.,0.,-1.));
#17848=DIRECTION('center_axis',(1.,0.,0.));
#17849=DIRECTION('ref_axis',(0.,0.,-1.));
#17850=DIRECTION('center_axis',(1.,0.,0.));
#17851=DIRECTION('ref_axis',(0.,0.,-1.));
#17852=DIRECTION('',(1.,0.,0.));
#17853=DIRECTION('center_axis',(-1.,0.,0.));
#17854=DIRECTION('ref_axis',(0.,0.,-1.));
#17855=DIRECTION('center_axis',(1.,0.,0.));
#17856=DIRECTION('ref_axis',(0.,0.,-1.));
#17857=DIRECTION('center_axis',(1.,0.,0.));
#17858=DIRECTION('ref_axis',(0.,0.,-1.));
#17859=DIRECTION('',(1.,0.,0.));
#17860=DIRECTION('center_axis',(-1.,0.,0.));
#17861=DIRECTION('ref_axis',(0.,0.,-1.));
#17862=DIRECTION('center_axis',(0.,1.,0.));
#17863=DIRECTION('ref_axis',(-1.,0.,0.));
#17864=DIRECTION('',(-1.,0.,0.));
#17865=DIRECTION('',(0.,0.,1.));
#17866=DIRECTION('',(-1.,0.,0.));
#17867=DIRECTION('',(0.,0.,1.));
#17868=DIRECTION('center_axis',(1.,0.,0.));
#17869=DIRECTION('ref_axis',(0.,1.,0.));
#17870=DIRECTION('',(0.,1.,0.));
#17871=DIRECTION('',(0.,1.,0.));
#17872=DIRECTION('',(0.,0.,1.));
#17873=DIRECTION('center_axis',(0.,-1.,0.));
#17874=DIRECTION('ref_axis',(1.,0.,0.));
#17875=DIRECTION('',(1.,0.,0.));
#17876=DIRECTION('',(1.,0.,0.));
#17877=DIRECTION('',(0.,0.,1.));
#17878=DIRECTION('center_axis',(-1.,0.,0.));
#17879=DIRECTION('ref_axis',(0.,-1.,0.));
#17880=DIRECTION('',(0.,-1.,0.));
#17881=DIRECTION('',(0.,-1.,0.));
#17882=DIRECTION('center_axis',(0.,0.,1.));
#17883=DIRECTION('ref_axis',(1.,0.,0.));
#17884=DIRECTION('center_axis',(0.,0.,1.));
#17885=DIRECTION('ref_axis',(1.,0.,0.));
#17886=DIRECTION('axis',(0.,0.,1.));
#17887=DIRECTION('refdir',(1.,0.,0.));
#17888=DIRECTION('center_axis',(1.,0.,0.));
#17889=DIRECTION('ref_axis',(0.,0.,-1.));
#17890=DIRECTION('center_axis',(1.,0.,0.));
#17891=DIRECTION('ref_axis',(0.,0.,-1.));
#17892=DIRECTION('',(-1.,0.,0.));
#17893=DIRECTION('center_axis',(-1.,0.,0.));
#17894=DIRECTION('ref_axis',(0.,0.,-1.));
#17895=DIRECTION('center_axis',(1.,0.,0.));
#17896=DIRECTION('ref_axis',(0.,0.,-1.));
#17897=DIRECTION('center_axis',(-1.,0.,0.));
#17898=DIRECTION('ref_axis',(0.,0.,-1.));
#17899=DIRECTION('center_axis',(1.,0.,0.));
#17900=DIRECTION('ref_axis',(0.,0.,-1.));
#17901=DIRECTION('center_axis',(1.,0.,0.));
#17902=DIRECTION('ref_axis',(0.,0.,-1.));
#17903=DIRECTION('',(-1.,0.,0.));
#17904=DIRECTION('center_axis',(-1.,0.,0.));
#17905=DIRECTION('ref_axis',(0.,0.,-1.));
#17906=DIRECTION('center_axis',(1.,0.,0.));
#17907=DIRECTION('ref_axis',(0.,0.,-1.));
#17908=DIRECTION('center_axis',(-1.,0.,0.));
#17909=DIRECTION('ref_axis',(0.,0.,-1.));
#17910=DIRECTION('center_axis',(1.,0.,0.));
#17911=DIRECTION('ref_axis',(0.,0.,-1.));
#17912=DIRECTION('center_axis',(1.,0.,0.));
#17913=DIRECTION('ref_axis',(0.,0.,-1.));
#17914=DIRECTION('',(1.,0.,0.));
#17915=DIRECTION('center_axis',(-1.,0.,0.));
#17916=DIRECTION('ref_axis',(0.,0.,-1.));
#17917=DIRECTION('center_axis',(1.,0.,0.));
#17918=DIRECTION('ref_axis',(0.,0.,-1.));
#17919=DIRECTION('center_axis',(1.,0.,0.));
#17920=DIRECTION('ref_axis',(0.,0.,-1.));
#17921=DIRECTION('',(1.,0.,0.));
#17922=DIRECTION('center_axis',(1.,0.,0.));
#17923=DIRECTION('ref_axis',(0.,0.,-1.));
#17924=DIRECTION('center_axis',(1.,0.,0.));
#17925=DIRECTION('ref_axis',(0.,0.,-1.));
#17926=DIRECTION('',(1.,0.,0.));
#17927=DIRECTION('center_axis',(0.,0.,1.));
#17928=DIRECTION('ref_axis',(0.,-1.,0.));
#17929=DIRECTION('',(0.,-1.,0.));
#17930=DIRECTION('',(1.,0.,0.));
#17931=DIRECTION('',(0.,-1.,0.));
#17932=DIRECTION('',(1.,0.,0.));
#17933=DIRECTION('center_axis',(0.,1.,0.));
#17934=DIRECTION('ref_axis',(0.,0.,1.));
#17935=DIRECTION('',(0.,0.,1.));
#17936=DIRECTION('',(0.,0.,1.));
#17937=DIRECTION('',(1.,0.,0.));
#17938=DIRECTION('center_axis',(0.,0.,-1.));
#17939=DIRECTION('ref_axis',(0.,1.,0.));
#17940=DIRECTION('',(0.,1.,0.));
#17941=DIRECTION('',(0.,1.,0.));
#17942=DIRECTION('',(1.,0.,0.));
#17943=DIRECTION('center_axis',(0.,-1.,0.));
#17944=DIRECTION('ref_axis',(0.,0.,-1.));
#17945=DIRECTION('',(0.,0.,-1.));
#17946=DIRECTION('',(0.,0.,-1.));
#17947=DIRECTION('center_axis',(1.,0.,0.));
#17948=DIRECTION('ref_axis',(0.,0.,-1.));
#17949=DIRECTION('center_axis',(1.,0.,0.));
#17950=DIRECTION('ref_axis',(0.,0.,-1.));
#17951=DIRECTION('axis',(0.,0.,1.));
#17952=DIRECTION('refdir',(1.,0.,0.));
#17953=DIRECTION('center_axis',(1.,0.,0.));
#17954=DIRECTION('ref_axis',(0.,0.,-1.));
#17955=DIRECTION('center_axis',(1.,0.,0.));
#17956=DIRECTION('ref_axis',(0.,0.,-1.));
#17957=DIRECTION('',(-1.,0.,0.));
#17958=DIRECTION('center_axis',(1.,0.,0.));
#17959=DIRECTION('ref_axis',(0.,0.,-1.));
#17960=DIRECTION('center_axis',(1.,0.,0.));
#17961=DIRECTION('ref_axis',(0.,0.,-1.));
#17962=DIRECTION('center_axis',(-1.,0.,0.));
#17963=DIRECTION('ref_axis',(0.,0.,-1.));
#17964=DIRECTION('center_axis',(1.,0.,0.));
#17965=DIRECTION('ref_axis',(0.,0.,-1.));
#17966=DIRECTION('center_axis',(1.,0.,0.));
#17967=DIRECTION('ref_axis',(0.,0.,-1.));
#17968=DIRECTION('',(-1.,0.,0.));
#17969=DIRECTION('center_axis',(1.,0.,0.));
#17970=DIRECTION('ref_axis',(0.,0.,-1.));
#17971=DIRECTION('center_axis',(1.,0.,0.));
#17972=DIRECTION('ref_axis',(0.,0.,-1.));
#17973=DIRECTION('center_axis',(-1.,0.,0.));
#17974=DIRECTION('ref_axis',(0.,0.,-1.));
#17975=DIRECTION('center_axis',(1.,0.,0.));
#17976=DIRECTION('ref_axis',(0.,0.,-1.));
#17977=DIRECTION('center_axis',(1.,0.,0.));
#17978=DIRECTION('ref_axis',(0.,0.,-1.));
#17979=DIRECTION('',(1.,0.,0.));
#17980=DIRECTION('center_axis',(-1.,0.,0.));
#17981=DIRECTION('ref_axis',(0.,0.,-1.));
#17982=DIRECTION('center_axis',(1.,0.,0.));
#17983=DIRECTION('ref_axis',(0.,0.,-1.));
#17984=DIRECTION('',(1.,0.,0.));
#17985=DIRECTION('center_axis',(-1.,0.,0.));
#17986=DIRECTION('ref_axis',(0.,0.,-1.));
#17987=DIRECTION('center_axis',(1.,0.,0.));
#17988=DIRECTION('ref_axis',(0.,0.,-1.));
#17989=DIRECTION('',(1.,0.,0.));
#17990=DIRECTION('center_axis',(-1.,0.,0.));
#17991=DIRECTION('ref_axis',(0.,0.,-1.));
#17992=DIRECTION('center_axis',(0.,0.,1.));
#17993=DIRECTION('ref_axis',(0.,-1.,0.));
#17994=DIRECTION('',(0.,-1.,0.));
#17995=DIRECTION('',(1.,0.,0.));
#17996=DIRECTION('',(0.,-1.,0.));
#17997=DIRECTION('',(1.,0.,0.));
#17998=DIRECTION('center_axis',(0.,1.,0.));
#17999=DIRECTION('ref_axis',(0.,0.,1.));
#18000=DIRECTION('',(0.,0.,1.));
#18001=DIRECTION('',(0.,0.,1.));
#18002=DIRECTION('',(1.,0.,0.));
#18003=DIRECTION('center_axis',(0.,0.,-1.));
#18004=DIRECTION('ref_axis',(0.,1.,0.));
#18005=DIRECTION('',(0.,1.,0.));
#18006=DIRECTION('',(0.,1.,0.));
#18007=DIRECTION('',(1.,0.,0.));
#18008=DIRECTION('center_axis',(0.,-1.,0.));
#18009=DIRECTION('ref_axis',(0.,0.,-1.));
#18010=DIRECTION('',(0.,0.,-1.));
#18011=DIRECTION('',(0.,0.,-1.));
#18012=DIRECTION('center_axis',(1.,0.,0.));
#18013=DIRECTION('ref_axis',(0.,0.,-1.));
#18014=DIRECTION('center_axis',(1.,0.,0.));
#18015=DIRECTION('ref_axis',(0.,0.,-1.));
#18016=DIRECTION('axis',(0.,0.,1.));
#18017=DIRECTION('refdir',(1.,0.,0.));
#18018=DIRECTION('center_axis',(1.,0.,0.));
#18019=DIRECTION('ref_axis',(0.,0.,-1.));
#18020=DIRECTION('',(0.,1.,0.));
#18021=DIRECTION('center_axis',(1.,0.,0.));
#18022=DIRECTION('ref_axis',(0.,0.,-1.));
#18023=DIRECTION('center_axis',(1.,0.,0.));
#18024=DIRECTION('ref_axis',(0.,0.,-1.));
#18025=DIRECTION('center_axis',(1.,0.,0.));
#18026=DIRECTION('ref_axis',(0.,0.,-1.));
#18027=DIRECTION('',(1.,0.,0.));
#18028=DIRECTION('center_axis',(-1.,0.,0.));
#18029=DIRECTION('ref_axis',(0.,0.,-1.));
#18030=DIRECTION('center_axis',(1.,0.,0.));
#18031=DIRECTION('ref_axis',(0.,0.,-1.));
#18032=DIRECTION('center_axis',(1.,0.,0.));
#18033=DIRECTION('ref_axis',(0.,0.,-1.));
#18034=DIRECTION('',(0.,-1.,0.));
#18035=DIRECTION('center_axis',(0.,1.,0.));
#18036=DIRECTION('ref_axis',(1.,0.,0.));
#18037=DIRECTION('center_axis',(0.,1.,0.));
#18038=DIRECTION('ref_axis',(1.,0.,0.));
#18039=DIRECTION('',(0.,1.,0.));
#18040=DIRECTION('center_axis',(0.,-1.,0.));
#18041=DIRECTION('ref_axis',(1.,0.,0.));
#18042=DIRECTION('center_axis',(0.,1.,0.));
#18043=DIRECTION('ref_axis',(-1.,0.,0.));
#18044=DIRECTION('',(-1.,0.,0.));
#18045=DIRECTION('',(0.,0.,1.));
#18046=DIRECTION('',(-1.,0.,0.));
#18047=DIRECTION('',(0.,0.,1.));
#18048=DIRECTION('center_axis',(1.,0.,0.));
#18049=DIRECTION('ref_axis',(0.,1.,0.));
#18050=DIRECTION('',(0.,1.,0.));
#18051=DIRECTION('',(0.,1.,0.));
#18052=DIRECTION('',(0.,0.,1.));
#18053=DIRECTION('center_axis',(0.,-1.,0.));
#18054=DIRECTION('ref_axis',(1.,0.,0.));
#18055=DIRECTION('',(1.,0.,0.));
#18056=DIRECTION('',(1.,0.,0.));
#18057=DIRECTION('',(0.,0.,1.));
#18058=DIRECTION('center_axis',(-1.,0.,0.));
#18059=DIRECTION('ref_axis',(0.,-1.,0.));
#18060=DIRECTION('',(0.,-1.,0.));
#18061=DIRECTION('',(0.,-1.,0.));
#18062=DIRECTION('center_axis',(0.,0.,1.));
#18063=DIRECTION('ref_axis',(1.,0.,0.));
#18064=DIRECTION('center_axis',(0.,0.,1.));
#18065=DIRECTION('ref_axis',(1.,0.,0.));
#18066=DIRECTION('axis',(0.,0.,1.));
#18067=DIRECTION('refdir',(1.,0.,0.));
#18068=DIRECTION('center_axis',(0.,1.,0.));
#18069=DIRECTION('ref_axis',(1.,0.,0.));
#18070=DIRECTION('center_axis',(0.,1.,0.));
#18071=DIRECTION('ref_axis',(1.,0.,0.));
#18072=DIRECTION('',(0.,1.,0.));
#18073=DIRECTION('center_axis',(0.,-1.,0.));
#18074=DIRECTION('ref_axis',(1.,0.,0.));
#18075=DIRECTION('center_axis',(0.,1.,0.));
#18076=DIRECTION('ref_axis',(1.,0.,0.));
#18077=DIRECTION('center_axis',(0.,1.,0.));
#18078=DIRECTION('ref_axis',(1.,0.,0.));
#18079=DIRECTION('center_axis',(0.,1.,0.));
#18080=DIRECTION('ref_axis',(1.,0.,0.));
#18081=DIRECTION('',(0.,1.,0.));
#18082=DIRECTION('center_axis',(0.,1.,0.));
#18083=DIRECTION('ref_axis',(1.,0.,0.));
#18084=DIRECTION('center_axis',(0.,1.,0.));
#18085=DIRECTION('ref_axis',(1.,0.,0.));
#18086=DIRECTION('center_axis',(0.,1.,0.));
#18087=DIRECTION('ref_axis',(1.,0.,0.));
#18088=DIRECTION('center_axis',(0.,1.,0.));
#18089=DIRECTION('ref_axis',(1.,0.,0.));
#18090=DIRECTION('',(0.,-1.,0.));
#18091=DIRECTION('center_axis',(0.,1.,0.));
#18092=DIRECTION('ref_axis',(1.,0.,0.));
#18093=DIRECTION('center_axis',(0.,1.,0.));
#18094=DIRECTION('ref_axis',(1.,0.,0.));
#18095=DIRECTION('center_axis',(0.,1.,0.));
#18096=DIRECTION('ref_axis',(1.,0.,0.));
#18097=DIRECTION('axis',(0.,0.,1.));
#18098=DIRECTION('refdir',(1.,0.,0.));
#18099=DIRECTION('center_axis',(0.,1.,0.));
#18100=DIRECTION('ref_axis',(1.,0.,0.));
#18101=DIRECTION('center_axis',(0.,-1.,0.));
#18102=DIRECTION('ref_axis',(1.,0.,0.));
#18103=DIRECTION('',(0.,-1.,0.));
#18104=DIRECTION('center_axis',(0.,-1.,0.));
#18105=DIRECTION('ref_axis',(1.,0.,0.));
#18106=DIRECTION('center_axis',(0.,1.,0.));
#18107=DIRECTION('ref_axis',(1.,0.,0.));
#18108=DIRECTION('center_axis',(0.,1.,0.));
#18109=DIRECTION('ref_axis',(1.,0.,0.));
#18110=DIRECTION('',(0.,-1.,0.));
#18111=DIRECTION('center_axis',(0.,1.,0.));
#18112=DIRECTION('ref_axis',(1.,0.,0.));
#18113=DIRECTION('center_axis',(0.,1.,0.));
#18114=DIRECTION('ref_axis',(1.,0.,0.));
#18115=DIRECTION('center_axis',(0.,1.,0.));
#18116=DIRECTION('ref_axis',(1.,0.,0.));
#18117=DIRECTION('axis',(0.,0.,1.));
#18118=DIRECTION('refdir',(1.,0.,0.));
#18119=DIRECTION('center_axis',(0.,1.,0.));
#18120=DIRECTION('ref_axis',(1.,0.,0.));
#18121=DIRECTION('center_axis',(0.,-1.,0.));
#18122=DIRECTION('ref_axis',(1.,0.,0.));
#18123=DIRECTION('',(0.,-1.,0.));
#18124=DIRECTION('center_axis',(0.,-1.,0.));
#18125=DIRECTION('ref_axis',(1.,0.,0.));
#18126=DIRECTION('center_axis',(0.,1.,0.));
#18127=DIRECTION('ref_axis',(1.,0.,0.));
#18128=DIRECTION('center_axis',(0.,1.,0.));
#18129=DIRECTION('ref_axis',(1.,0.,0.));
#18130=DIRECTION('',(0.,-1.,0.));
#18131=DIRECTION('center_axis',(0.,1.,0.));
#18132=DIRECTION('ref_axis',(1.,0.,0.));
#18133=DIRECTION('center_axis',(0.,1.,0.));
#18134=DIRECTION('ref_axis',(1.,0.,0.));
#18135=DIRECTION('center_axis',(0.,1.,0.));
#18136=DIRECTION('ref_axis',(1.,0.,0.));
#18137=DIRECTION('axis',(0.,0.,1.));
#18138=DIRECTION('refdir',(1.,0.,0.));
#18139=DIRECTION('center_axis',(0.,1.,0.));
#18140=DIRECTION('ref_axis',(1.,0.,0.));
#18141=DIRECTION('center_axis',(0.,-1.,0.));
#18142=DIRECTION('ref_axis',(1.,0.,0.));
#18143=DIRECTION('',(0.,-1.,0.));
#18144=DIRECTION('center_axis',(0.,-1.,0.));
#18145=DIRECTION('ref_axis',(1.,0.,0.));
#18146=DIRECTION('center_axis',(0.,1.,0.));
#18147=DIRECTION('ref_axis',(1.,0.,0.));
#18148=DIRECTION('center_axis',(0.,1.,0.));
#18149=DIRECTION('ref_axis',(1.,0.,0.));
#18150=DIRECTION('',(0.,-1.,0.));
#18151=DIRECTION('center_axis',(0.,1.,0.));
#18152=DIRECTION('ref_axis',(1.,0.,0.));
#18153=DIRECTION('center_axis',(0.,1.,0.));
#18154=DIRECTION('ref_axis',(1.,0.,0.));
#18155=DIRECTION('center_axis',(0.,1.,0.));
#18156=DIRECTION('ref_axis',(1.,0.,0.));
#18157=DIRECTION('axis',(0.,0.,1.));
#18158=DIRECTION('refdir',(1.,0.,0.));
#18159=DIRECTION('center_axis',(0.,1.,0.));
#18160=DIRECTION('ref_axis',(1.,0.,0.));
#18161=DIRECTION('center_axis',(0.,-1.,0.));
#18162=DIRECTION('ref_axis',(1.,0.,0.));
#18163=DIRECTION('',(0.,-1.,0.));
#18164=DIRECTION('center_axis',(0.,-1.,0.));
#18165=DIRECTION('ref_axis',(1.,0.,0.));
#18166=DIRECTION('center_axis',(0.,1.,0.));
#18167=DIRECTION('ref_axis',(1.,0.,0.));
#18168=DIRECTION('center_axis',(0.,1.,0.));
#18169=DIRECTION('ref_axis',(1.,0.,0.));
#18170=DIRECTION('',(0.,-1.,0.));
#18171=DIRECTION('center_axis',(0.,1.,0.));
#18172=DIRECTION('ref_axis',(1.,0.,0.));
#18173=DIRECTION('center_axis',(0.,1.,0.));
#18174=DIRECTION('ref_axis',(1.,0.,0.));
#18175=DIRECTION('center_axis',(0.,1.,0.));
#18176=DIRECTION('ref_axis',(1.,0.,0.));
#18177=DIRECTION('axis',(0.,0.,1.));
#18178=DIRECTION('refdir',(1.,0.,0.));
#18179=DIRECTION('center_axis',(0.,1.,0.));
#18180=DIRECTION('ref_axis',(1.,0.,0.));
#18181=DIRECTION('center_axis',(0.,-1.,0.));
#18182=DIRECTION('ref_axis',(1.,0.,0.));
#18183=DIRECTION('',(0.,-1.,0.));
#18184=DIRECTION('center_axis',(0.,-1.,0.));
#18185=DIRECTION('ref_axis',(1.,0.,0.));
#18186=DIRECTION('center_axis',(0.,1.,0.));
#18187=DIRECTION('ref_axis',(1.,0.,0.));
#18188=DIRECTION('center_axis',(0.,1.,0.));
#18189=DIRECTION('ref_axis',(1.,0.,0.));
#18190=DIRECTION('',(0.,-1.,0.));
#18191=DIRECTION('center_axis',(0.,1.,0.));
#18192=DIRECTION('ref_axis',(1.,0.,0.));
#18193=DIRECTION('center_axis',(0.,1.,0.));
#18194=DIRECTION('ref_axis',(1.,0.,0.));
#18195=DIRECTION('center_axis',(0.,1.,0.));
#18196=DIRECTION('ref_axis',(1.,0.,0.));
#18197=DIRECTION('axis',(0.,0.,1.));
#18198=DIRECTION('refdir',(1.,0.,0.));
#18199=DIRECTION('center_axis',(0.,1.,0.));
#18200=DIRECTION('ref_axis',(1.,0.,0.));
#18201=DIRECTION('center_axis',(0.,-1.,0.));
#18202=DIRECTION('ref_axis',(1.,0.,0.));
#18203=DIRECTION('',(0.,-1.,0.));
#18204=DIRECTION('center_axis',(0.,-1.,0.));
#18205=DIRECTION('ref_axis',(1.,0.,0.));
#18206=DIRECTION('center_axis',(0.,1.,0.));
#18207=DIRECTION('ref_axis',(1.,0.,0.));
#18208=DIRECTION('center_axis',(0.,1.,0.));
#18209=DIRECTION('ref_axis',(1.,0.,0.));
#18210=DIRECTION('',(0.,-1.,0.));
#18211=DIRECTION('center_axis',(0.,1.,0.));
#18212=DIRECTION('ref_axis',(1.,0.,0.));
#18213=DIRECTION('center_axis',(0.,1.,0.));
#18214=DIRECTION('ref_axis',(1.,0.,0.));
#18215=DIRECTION('center_axis',(0.,1.,0.));
#18216=DIRECTION('ref_axis',(1.,0.,0.));
#18217=DIRECTION('axis',(0.,0.,1.));
#18218=DIRECTION('refdir',(1.,0.,0.));
#18219=DIRECTION('axis',(0.,0.,1.));
#18220=DIRECTION('refdir',(1.,0.,0.));
#18221=DIRECTION('center_axis',(1.,0.,0.));
#18222=DIRECTION('ref_axis',(0.,0.,-1.));
#18223=DIRECTION('center_axis',(1.,0.,0.));
#18224=DIRECTION('ref_axis',(0.,0.,-1.));
#18225=DIRECTION('',(1.,0.,0.));
#18226=DIRECTION('center_axis',(-1.,0.,0.));
#18227=DIRECTION('ref_axis',(0.,0.,-1.));
#18228=DIRECTION('center_axis',(1.,0.,0.));
#18229=DIRECTION('ref_axis',(0.,0.,-1.));
#18230=DIRECTION('center_axis',(1.,0.,0.));
#18231=DIRECTION('ref_axis',(0.,0.,-1.));
#18232=DIRECTION('',(1.,0.,0.));
#18233=DIRECTION('center_axis',(-1.,0.,0.));
#18234=DIRECTION('ref_axis',(0.,0.,-1.));
#18235=DIRECTION('center_axis',(1.,0.,0.));
#18236=DIRECTION('ref_axis',(0.,0.,-1.));
#18237=DIRECTION('center_axis',(1.,0.,0.));
#18238=DIRECTION('ref_axis',(0.,0.,-1.));
#18239=DIRECTION('',(1.,0.,0.));
#18240=DIRECTION('center_axis',(-1.,0.,0.));
#18241=DIRECTION('ref_axis',(0.,0.,-1.));
#18242=DIRECTION('center_axis',(0.,1.,0.));
#18243=DIRECTION('ref_axis',(-1.,0.,0.));
#18244=DIRECTION('',(-1.,0.,0.));
#18245=DIRECTION('',(0.,0.,1.));
#18246=DIRECTION('',(-1.,0.,0.));
#18247=DIRECTION('',(0.,0.,1.));
#18248=DIRECTION('center_axis',(1.,0.,0.));
#18249=DIRECTION('ref_axis',(0.,1.,0.));
#18250=DIRECTION('',(0.,1.,0.));
#18251=DIRECTION('',(0.,1.,0.));
#18252=DIRECTION('',(0.,0.,1.));
#18253=DIRECTION('center_axis',(0.,-1.,0.));
#18254=DIRECTION('ref_axis',(1.,0.,0.));
#18255=DIRECTION('',(1.,0.,0.));
#18256=DIRECTION('',(1.,0.,0.));
#18257=DIRECTION('',(0.,0.,1.));
#18258=DIRECTION('center_axis',(-1.,0.,0.));
#18259=DIRECTION('ref_axis',(0.,-1.,0.));
#18260=DIRECTION('',(0.,-1.,0.));
#18261=DIRECTION('',(0.,-1.,0.));
#18262=DIRECTION('center_axis',(0.,0.,1.));
#18263=DIRECTION('ref_axis',(1.,0.,0.));
#18264=DIRECTION('center_axis',(0.,0.,1.));
#18265=DIRECTION('ref_axis',(1.,0.,0.));
#18266=DIRECTION('axis',(0.,0.,1.));
#18267=DIRECTION('refdir',(1.,0.,0.));
#18268=DIRECTION('center_axis',(1.,0.,0.));
#18269=DIRECTION('ref_axis',(0.,0.,-1.));
#18270=DIRECTION('center_axis',(1.,0.,0.));
#18271=DIRECTION('ref_axis',(0.,0.,-1.));
#18272=DIRECTION('',(-1.,0.,0.));
#18273=DIRECTION('center_axis',(-1.,0.,0.));
#18274=DIRECTION('ref_axis',(0.,0.,-1.));
#18275=DIRECTION('center_axis',(1.,0.,0.));
#18276=DIRECTION('ref_axis',(0.,0.,-1.));
#18277=DIRECTION('center_axis',(-1.,0.,0.));
#18278=DIRECTION('ref_axis',(0.,0.,-1.));
#18279=DIRECTION('center_axis',(1.,0.,0.));
#18280=DIRECTION('ref_axis',(0.,0.,-1.));
#18281=DIRECTION('center_axis',(1.,0.,0.));
#18282=DIRECTION('ref_axis',(0.,0.,-1.));
#18283=DIRECTION('',(-1.,0.,0.));
#18284=DIRECTION('center_axis',(-1.,0.,0.));
#18285=DIRECTION('ref_axis',(0.,0.,-1.));
#18286=DIRECTION('center_axis',(1.,0.,0.));
#18287=DIRECTION('ref_axis',(0.,0.,-1.));
#18288=DIRECTION('center_axis',(-1.,0.,0.));
#18289=DIRECTION('ref_axis',(0.,0.,-1.));
#18290=DIRECTION('center_axis',(1.,0.,0.));
#18291=DIRECTION('ref_axis',(0.,0.,-1.));
#18292=DIRECTION('center_axis',(1.,0.,0.));
#18293=DIRECTION('ref_axis',(0.,0.,-1.));
#18294=DIRECTION('',(1.,0.,0.));
#18295=DIRECTION('center_axis',(-1.,0.,0.));
#18296=DIRECTION('ref_axis',(0.,0.,-1.));
#18297=DIRECTION('center_axis',(1.,0.,0.));
#18298=DIRECTION('ref_axis',(0.,0.,-1.));
#18299=DIRECTION('center_axis',(1.,0.,0.));
#18300=DIRECTION('ref_axis',(0.,0.,-1.));
#18301=DIRECTION('',(1.,0.,0.));
#18302=DIRECTION('center_axis',(1.,0.,0.));
#18303=DIRECTION('ref_axis',(0.,0.,-1.));
#18304=DIRECTION('center_axis',(1.,0.,0.));
#18305=DIRECTION('ref_axis',(0.,0.,-1.));
#18306=DIRECTION('',(1.,0.,0.));
#18307=DIRECTION('center_axis',(0.,0.,1.));
#18308=DIRECTION('ref_axis',(0.,-1.,0.));
#18309=DIRECTION('',(0.,-1.,0.));
#18310=DIRECTION('',(1.,0.,0.));
#18311=DIRECTION('',(0.,-1.,0.));
#18312=DIRECTION('',(1.,0.,0.));
#18313=DIRECTION('center_axis',(0.,1.,0.));
#18314=DIRECTION('ref_axis',(0.,0.,1.));
#18315=DIRECTION('',(0.,0.,1.));
#18316=DIRECTION('',(0.,0.,1.));
#18317=DIRECTION('',(1.,0.,0.));
#18318=DIRECTION('center_axis',(0.,0.,-1.));
#18319=DIRECTION('ref_axis',(0.,1.,0.));
#18320=DIRECTION('',(0.,1.,0.));
#18321=DIRECTION('',(0.,1.,0.));
#18322=DIRECTION('',(1.,0.,0.));
#18323=DIRECTION('center_axis',(0.,-1.,0.));
#18324=DIRECTION('ref_axis',(0.,0.,-1.));
#18325=DIRECTION('',(0.,0.,-1.));
#18326=DIRECTION('',(0.,0.,-1.));
#18327=DIRECTION('center_axis',(1.,0.,0.));
#18328=DIRECTION('ref_axis',(0.,0.,-1.));
#18329=DIRECTION('center_axis',(1.,0.,0.));
#18330=DIRECTION('ref_axis',(0.,0.,-1.));
#18331=DIRECTION('axis',(0.,0.,1.));
#18332=DIRECTION('refdir',(1.,0.,0.));
#18333=DIRECTION('center_axis',(1.,0.,0.));
#18334=DIRECTION('ref_axis',(0.,0.,-1.));
#18335=DIRECTION('center_axis',(1.,0.,0.));
#18336=DIRECTION('ref_axis',(0.,0.,-1.));
#18337=DIRECTION('',(-1.,0.,0.));
#18338=DIRECTION('center_axis',(1.,0.,0.));
#18339=DIRECTION('ref_axis',(0.,0.,-1.));
#18340=DIRECTION('center_axis',(1.,0.,0.));
#18341=DIRECTION('ref_axis',(0.,0.,-1.));
#18342=DIRECTION('center_axis',(-1.,0.,0.));
#18343=DIRECTION('ref_axis',(0.,0.,-1.));
#18344=DIRECTION('center_axis',(1.,0.,0.));
#18345=DIRECTION('ref_axis',(0.,0.,-1.));
#18346=DIRECTION('center_axis',(1.,0.,0.));
#18347=DIRECTION('ref_axis',(0.,0.,-1.));
#18348=DIRECTION('',(-1.,0.,0.));
#18349=DIRECTION('center_axis',(1.,0.,0.));
#18350=DIRECTION('ref_axis',(0.,0.,-1.));
#18351=DIRECTION('center_axis',(1.,0.,0.));
#18352=DIRECTION('ref_axis',(0.,0.,-1.));
#18353=DIRECTION('center_axis',(-1.,0.,0.));
#18354=DIRECTION('ref_axis',(0.,0.,-1.));
#18355=DIRECTION('center_axis',(1.,0.,0.));
#18356=DIRECTION('ref_axis',(0.,0.,-1.));
#18357=DIRECTION('center_axis',(1.,0.,0.));
#18358=DIRECTION('ref_axis',(0.,0.,-1.));
#18359=DIRECTION('',(1.,0.,0.));
#18360=DIRECTION('center_axis',(-1.,0.,0.));
#18361=DIRECTION('ref_axis',(0.,0.,-1.));
#18362=DIRECTION('center_axis',(1.,0.,0.));
#18363=DIRECTION('ref_axis',(0.,0.,-1.));
#18364=DIRECTION('',(1.,0.,0.));
#18365=DIRECTION('center_axis',(-1.,0.,0.));
#18366=DIRECTION('ref_axis',(0.,0.,-1.));
#18367=DIRECTION('center_axis',(1.,0.,0.));
#18368=DIRECTION('ref_axis',(0.,0.,-1.));
#18369=DIRECTION('',(1.,0.,0.));
#18370=DIRECTION('center_axis',(-1.,0.,0.));
#18371=DIRECTION('ref_axis',(0.,0.,-1.));
#18372=DIRECTION('center_axis',(0.,0.,1.));
#18373=DIRECTION('ref_axis',(0.,-1.,0.));
#18374=DIRECTION('',(0.,-1.,0.));
#18375=DIRECTION('',(1.,0.,0.));
#18376=DIRECTION('',(0.,-1.,0.));
#18377=DIRECTION('',(1.,0.,0.));
#18378=DIRECTION('center_axis',(0.,1.,0.));
#18379=DIRECTION('ref_axis',(0.,0.,1.));
#18380=DIRECTION('',(0.,0.,1.));
#18381=DIRECTION('',(0.,0.,1.));
#18382=DIRECTION('',(1.,0.,0.));
#18383=DIRECTION('center_axis',(0.,0.,-1.));
#18384=DIRECTION('ref_axis',(0.,1.,0.));
#18385=DIRECTION('',(0.,1.,0.));
#18386=DIRECTION('',(0.,1.,0.));
#18387=DIRECTION('',(1.,0.,0.));
#18388=DIRECTION('center_axis',(0.,-1.,0.));
#18389=DIRECTION('ref_axis',(0.,0.,-1.));
#18390=DIRECTION('',(0.,0.,-1.));
#18391=DIRECTION('',(0.,0.,-1.));
#18392=DIRECTION('center_axis',(1.,0.,0.));
#18393=DIRECTION('ref_axis',(0.,0.,-1.));
#18394=DIRECTION('center_axis',(1.,0.,0.));
#18395=DIRECTION('ref_axis',(0.,0.,-1.));
#18396=DIRECTION('axis',(0.,0.,1.));
#18397=DIRECTION('refdir',(1.,0.,0.));
#18398=DIRECTION('center_axis',(1.,0.,0.));
#18399=DIRECTION('ref_axis',(0.,0.,-1.));
#18400=DIRECTION('',(0.,1.,0.));
#18401=DIRECTION('center_axis',(1.,0.,0.));
#18402=DIRECTION('ref_axis',(0.,0.,-1.));
#18403=DIRECTION('center_axis',(1.,0.,0.));
#18404=DIRECTION('ref_axis',(0.,0.,-1.));
#18405=DIRECTION('center_axis',(1.,0.,0.));
#18406=DIRECTION('ref_axis',(0.,0.,-1.));
#18407=DIRECTION('',(1.,0.,0.));
#18408=DIRECTION('center_axis',(-1.,0.,0.));
#18409=DIRECTION('ref_axis',(0.,0.,-1.));
#18410=DIRECTION('center_axis',(1.,0.,0.));
#18411=DIRECTION('ref_axis',(0.,0.,-1.));
#18412=DIRECTION('center_axis',(1.,0.,0.));
#18413=DIRECTION('ref_axis',(0.,0.,-1.));
#18414=DIRECTION('',(0.,-1.,0.));
#18415=DIRECTION('center_axis',(0.,1.,0.));
#18416=DIRECTION('ref_axis',(1.,0.,0.));
#18417=DIRECTION('center_axis',(0.,1.,0.));
#18418=DIRECTION('ref_axis',(1.,0.,0.));
#18419=DIRECTION('',(0.,1.,0.));
#18420=DIRECTION('center_axis',(0.,-1.,0.));
#18421=DIRECTION('ref_axis',(1.,0.,0.));
#18422=DIRECTION('center_axis',(0.,1.,0.));
#18423=DIRECTION('ref_axis',(-1.,0.,0.));
#18424=DIRECTION('',(-1.,0.,0.));
#18425=DIRECTION('',(0.,0.,1.));
#18426=DIRECTION('',(-1.,0.,0.));
#18427=DIRECTION('',(0.,0.,1.));
#18428=DIRECTION('center_axis',(1.,0.,0.));
#18429=DIRECTION('ref_axis',(0.,1.,0.));
#18430=DIRECTION('',(0.,1.,0.));
#18431=DIRECTION('',(0.,1.,0.));
#18432=DIRECTION('',(0.,0.,1.));
#18433=DIRECTION('center_axis',(0.,-1.,0.));
#18434=DIRECTION('ref_axis',(1.,0.,0.));
#18435=DIRECTION('',(1.,0.,0.));
#18436=DIRECTION('',(1.,0.,0.));
#18437=DIRECTION('',(0.,0.,1.));
#18438=DIRECTION('center_axis',(-1.,0.,0.));
#18439=DIRECTION('ref_axis',(0.,-1.,0.));
#18440=DIRECTION('',(0.,-1.,0.));
#18441=DIRECTION('',(0.,-1.,0.));
#18442=DIRECTION('center_axis',(0.,0.,1.));
#18443=DIRECTION('ref_axis',(1.,0.,0.));
#18444=DIRECTION('center_axis',(0.,0.,1.));
#18445=DIRECTION('ref_axis',(1.,0.,0.));
#18446=DIRECTION('axis',(0.,0.,1.));
#18447=DIRECTION('refdir',(1.,0.,0.));
#18448=DIRECTION('center_axis',(0.,1.,0.));
#18449=DIRECTION('ref_axis',(1.,0.,0.));
#18450=DIRECTION('center_axis',(0.,1.,0.));
#18451=DIRECTION('ref_axis',(1.,0.,0.));
#18452=DIRECTION('',(0.,1.,0.));
#18453=DIRECTION('center_axis',(0.,-1.,0.));
#18454=DIRECTION('ref_axis',(1.,0.,0.));
#18455=DIRECTION('center_axis',(0.,1.,0.));
#18456=DIRECTION('ref_axis',(1.,0.,0.));
#18457=DIRECTION('center_axis',(0.,1.,0.));
#18458=DIRECTION('ref_axis',(1.,0.,0.));
#18459=DIRECTION('center_axis',(0.,1.,0.));
#18460=DIRECTION('ref_axis',(1.,0.,0.));
#18461=DIRECTION('',(0.,1.,0.));
#18462=DIRECTION('center_axis',(0.,1.,0.));
#18463=DIRECTION('ref_axis',(1.,0.,0.));
#18464=DIRECTION('center_axis',(0.,1.,0.));
#18465=DIRECTION('ref_axis',(1.,0.,0.));
#18466=DIRECTION('center_axis',(0.,1.,0.));
#18467=DIRECTION('ref_axis',(1.,0.,0.));
#18468=DIRECTION('center_axis',(0.,1.,0.));
#18469=DIRECTION('ref_axis',(1.,0.,0.));
#18470=DIRECTION('',(0.,-1.,0.));
#18471=DIRECTION('center_axis',(0.,1.,0.));
#18472=DIRECTION('ref_axis',(1.,0.,0.));
#18473=DIRECTION('center_axis',(0.,1.,0.));
#18474=DIRECTION('ref_axis',(1.,0.,0.));
#18475=DIRECTION('center_axis',(0.,1.,0.));
#18476=DIRECTION('ref_axis',(1.,0.,0.));
#18477=DIRECTION('axis',(0.,0.,1.));
#18478=DIRECTION('refdir',(1.,0.,0.));
#18479=DIRECTION('center_axis',(0.,1.,0.));
#18480=DIRECTION('ref_axis',(1.,0.,0.));
#18481=DIRECTION('center_axis',(0.,-1.,0.));
#18482=DIRECTION('ref_axis',(1.,0.,0.));
#18483=DIRECTION('',(0.,-1.,0.));
#18484=DIRECTION('center_axis',(0.,-1.,0.));
#18485=DIRECTION('ref_axis',(1.,0.,0.));
#18486=DIRECTION('center_axis',(0.,1.,0.));
#18487=DIRECTION('ref_axis',(1.,0.,0.));
#18488=DIRECTION('center_axis',(0.,1.,0.));
#18489=DIRECTION('ref_axis',(1.,0.,0.));
#18490=DIRECTION('',(0.,-1.,0.));
#18491=DIRECTION('center_axis',(0.,1.,0.));
#18492=DIRECTION('ref_axis',(1.,0.,0.));
#18493=DIRECTION('center_axis',(0.,1.,0.));
#18494=DIRECTION('ref_axis',(1.,0.,0.));
#18495=DIRECTION('center_axis',(0.,1.,0.));
#18496=DIRECTION('ref_axis',(1.,0.,0.));
#18497=DIRECTION('axis',(0.,0.,1.));
#18498=DIRECTION('refdir',(1.,0.,0.));
#18499=DIRECTION('center_axis',(0.,1.,0.));
#18500=DIRECTION('ref_axis',(1.,0.,0.));
#18501=DIRECTION('center_axis',(0.,-1.,0.));
#18502=DIRECTION('ref_axis',(1.,0.,0.));
#18503=DIRECTION('',(0.,-1.,0.));
#18504=DIRECTION('center_axis',(0.,-1.,0.));
#18505=DIRECTION('ref_axis',(1.,0.,0.));
#18506=DIRECTION('center_axis',(0.,1.,0.));
#18507=DIRECTION('ref_axis',(1.,0.,0.));
#18508=DIRECTION('center_axis',(0.,1.,0.));
#18509=DIRECTION('ref_axis',(1.,0.,0.));
#18510=DIRECTION('',(0.,-1.,0.));
#18511=DIRECTION('center_axis',(0.,1.,0.));
#18512=DIRECTION('ref_axis',(1.,0.,0.));
#18513=DIRECTION('center_axis',(0.,1.,0.));
#18514=DIRECTION('ref_axis',(1.,0.,0.));
#18515=DIRECTION('center_axis',(0.,1.,0.));
#18516=DIRECTION('ref_axis',(1.,0.,0.));
#18517=DIRECTION('axis',(0.,0.,1.));
#18518=DIRECTION('refdir',(1.,0.,0.));
#18519=DIRECTION('center_axis',(0.,1.,0.));
#18520=DIRECTION('ref_axis',(1.,0.,0.));
#18521=DIRECTION('center_axis',(0.,-1.,0.));
#18522=DIRECTION('ref_axis',(1.,0.,0.));
#18523=DIRECTION('',(0.,-1.,0.));
#18524=DIRECTION('center_axis',(0.,-1.,0.));
#18525=DIRECTION('ref_axis',(1.,0.,0.));
#18526=DIRECTION('center_axis',(0.,1.,0.));
#18527=DIRECTION('ref_axis',(1.,0.,0.));
#18528=DIRECTION('center_axis',(0.,1.,0.));
#18529=DIRECTION('ref_axis',(1.,0.,0.));
#18530=DIRECTION('',(0.,-1.,0.));
#18531=DIRECTION('center_axis',(0.,1.,0.));
#18532=DIRECTION('ref_axis',(1.,0.,0.));
#18533=DIRECTION('center_axis',(0.,1.,0.));
#18534=DIRECTION('ref_axis',(1.,0.,0.));
#18535=DIRECTION('center_axis',(0.,1.,0.));
#18536=DIRECTION('ref_axis',(1.,0.,0.));
#18537=DIRECTION('axis',(0.,0.,1.));
#18538=DIRECTION('refdir',(1.,0.,0.));
#18539=DIRECTION('center_axis',(0.,1.,0.));
#18540=DIRECTION('ref_axis',(1.,0.,0.));
#18541=DIRECTION('center_axis',(0.,-1.,0.));
#18542=DIRECTION('ref_axis',(1.,0.,0.));
#18543=DIRECTION('',(0.,-1.,0.));
#18544=DIRECTION('center_axis',(0.,-1.,0.));
#18545=DIRECTION('ref_axis',(1.,0.,0.));
#18546=DIRECTION('center_axis',(0.,1.,0.));
#18547=DIRECTION('ref_axis',(1.,0.,0.));
#18548=DIRECTION('center_axis',(0.,1.,0.));
#18549=DIRECTION('ref_axis',(1.,0.,0.));
#18550=DIRECTION('',(0.,-1.,0.));
#18551=DIRECTION('center_axis',(0.,1.,0.));
#18552=DIRECTION('ref_axis',(1.,0.,0.));
#18553=DIRECTION('center_axis',(0.,1.,0.));
#18554=DIRECTION('ref_axis',(1.,0.,0.));
#18555=DIRECTION('center_axis',(0.,1.,0.));
#18556=DIRECTION('ref_axis',(1.,0.,0.));
#18557=DIRECTION('axis',(0.,0.,1.));
#18558=DIRECTION('refdir',(1.,0.,0.));
#18559=DIRECTION('center_axis',(0.,1.,0.));
#18560=DIRECTION('ref_axis',(1.,0.,0.));
#18561=DIRECTION('center_axis',(0.,-1.,0.));
#18562=DIRECTION('ref_axis',(1.,0.,0.));
#18563=DIRECTION('',(0.,-1.,0.));
#18564=DIRECTION('center_axis',(0.,-1.,0.));
#18565=DIRECTION('ref_axis',(1.,0.,0.));
#18566=DIRECTION('center_axis',(0.,1.,0.));
#18567=DIRECTION('ref_axis',(1.,0.,0.));
#18568=DIRECTION('center_axis',(0.,1.,0.));
#18569=DIRECTION('ref_axis',(1.,0.,0.));
#18570=DIRECTION('',(0.,-1.,0.));
#18571=DIRECTION('center_axis',(0.,1.,0.));
#18572=DIRECTION('ref_axis',(1.,0.,0.));
#18573=DIRECTION('center_axis',(0.,1.,0.));
#18574=DIRECTION('ref_axis',(1.,0.,0.));
#18575=DIRECTION('center_axis',(0.,1.,0.));
#18576=DIRECTION('ref_axis',(1.,0.,0.));
#18577=DIRECTION('axis',(0.,0.,1.));
#18578=DIRECTION('refdir',(1.,0.,0.));
#18579=DIRECTION('center_axis',(0.,1.,0.));
#18580=DIRECTION('ref_axis',(1.,0.,0.));
#18581=DIRECTION('center_axis',(0.,-1.,0.));
#18582=DIRECTION('ref_axis',(1.,0.,0.));
#18583=DIRECTION('',(0.,-1.,0.));
#18584=DIRECTION('center_axis',(0.,-1.,0.));
#18585=DIRECTION('ref_axis',(1.,0.,0.));
#18586=DIRECTION('center_axis',(0.,1.,0.));
#18587=DIRECTION('ref_axis',(1.,0.,0.));
#18588=DIRECTION('center_axis',(0.,1.,0.));
#18589=DIRECTION('ref_axis',(1.,0.,0.));
#18590=DIRECTION('',(0.,-1.,0.));
#18591=DIRECTION('center_axis',(0.,1.,0.));
#18592=DIRECTION('ref_axis',(1.,0.,0.));
#18593=DIRECTION('center_axis',(0.,1.,0.));
#18594=DIRECTION('ref_axis',(1.,0.,0.));
#18595=DIRECTION('center_axis',(0.,1.,0.));
#18596=DIRECTION('ref_axis',(1.,0.,0.));
#18597=DIRECTION('axis',(0.,0.,1.));
#18598=DIRECTION('refdir',(1.,0.,0.));
#18599=DIRECTION('axis',(0.,0.,1.));
#18600=DIRECTION('refdir',(1.,0.,0.));
#18601=DIRECTION('center_axis',(0.,1.,0.));
#18602=DIRECTION('ref_axis',(0.,0.,1.));
#18603=DIRECTION('center_axis',(0.,-1.,0.));
#18604=DIRECTION('ref_axis',(1.,0.,0.));
#18605=DIRECTION('',(-1.,0.,0.));
#18606=DIRECTION('',(0.,0.,-1.));
#18607=DIRECTION('',(1.,0.,0.));
#18608=DIRECTION('center_axis',(0.,0.,1.));
#18609=DIRECTION('ref_axis',(1.,0.,0.));
#18610=DIRECTION('',(0.,-1.,0.));
#18611=DIRECTION('',(0.,1.,0.));
#18612=DIRECTION('',(-1.,0.,0.));
#18613=DIRECTION('center_axis',(0.,-1.,0.));
#18614=DIRECTION('ref_axis',(0.,0.,-1.));
#18615=DIRECTION('center_axis',(0.,1.,0.));
#18616=DIRECTION('ref_axis',(1.,0.,0.));
#18617=DIRECTION('',(0.,0.,1.));
#18618=DIRECTION('',(1.,0.,0.));
#18619=DIRECTION('center_axis',(0.,0.,-1.));
#18620=DIRECTION('ref_axis',(-1.,0.,0.));
#18621=DIRECTION('',(0.,1.,0.));
#18622=DIRECTION('',(0.,1.,0.));
#18623=DIRECTION('center_axis',(1.,0.,0.));
#18624=DIRECTION('ref_axis',(0.,0.,-1.));
#18625=DIRECTION('center_axis',(0.,1.,0.));
#18626=DIRECTION('ref_axis',(0.,0.,1.));
#18627=DIRECTION('center_axis',(0.,-1.,0.));
#18628=DIRECTION('ref_axis',(1.,0.,0.));
#18629=DIRECTION('center_axis',(0.,-1.,0.));
#18630=DIRECTION('ref_axis',(1.,0.,0.));
#18631=DIRECTION('center_axis',(0.,-1.,0.));
#18632=DIRECTION('ref_axis',(1.,0.,0.));
#18633=DIRECTION('center_axis',(0.,-1.,0.));
#18634=DIRECTION('ref_axis',(1.,0.,0.));
#18635=DIRECTION('',(0.,1.,0.));
#18636=DIRECTION('center_axis',(0.,-1.,0.));
#18637=DIRECTION('ref_axis',(0.,0.,-1.));
#18638=DIRECTION('center_axis',(0.,-1.,0.));
#18639=DIRECTION('ref_axis',(1.,0.,0.));
#18640=DIRECTION('center_axis',(0.,-1.,0.));
#18641=DIRECTION('ref_axis',(1.,0.,0.));
#18642=DIRECTION('center_axis',(0.,-1.,0.));
#18643=DIRECTION('ref_axis',(1.,0.,0.));
#18644=DIRECTION('',(0.,1.,0.));
#18645=DIRECTION('center_axis',(0.,1.,0.));
#18646=DIRECTION('ref_axis',(0.,0.,1.));
#18647=DIRECTION('center_axis',(0.,-1.,0.));
#18648=DIRECTION('ref_axis',(1.,0.,0.));
#18649=DIRECTION('center_axis',(0.,-1.,0.));
#18650=DIRECTION('ref_axis',(1.,0.,0.));
#18651=DIRECTION('center_axis',(0.,-1.,0.));
#18652=DIRECTION('ref_axis',(1.,0.,0.));
#18653=DIRECTION('',(0.,1.,0.));
#18654=DIRECTION('center_axis',(0.,-1.,0.));
#18655=DIRECTION('ref_axis',(0.,0.,-1.));
#18656=DIRECTION('center_axis',(0.,-1.,0.));
#18657=DIRECTION('ref_axis',(1.,0.,0.));
#18658=DIRECTION('center_axis',(0.,-1.,0.));
#18659=DIRECTION('ref_axis',(1.,0.,0.));
#18660=DIRECTION('center_axis',(0.,-1.,0.));
#18661=DIRECTION('ref_axis',(1.,0.,0.));
#18662=DIRECTION('',(0.,1.,0.));
#18663=DIRECTION('center_axis',(0.,1.,0.));
#18664=DIRECTION('ref_axis',(0.,0.,1.));
#18665=DIRECTION('center_axis',(0.,-1.,0.));
#18666=DIRECTION('ref_axis',(1.,0.,0.));
#18667=DIRECTION('center_axis',(0.,-1.,0.));
#18668=DIRECTION('ref_axis',(1.,0.,0.));
#18669=DIRECTION('center_axis',(0.,-1.,0.));
#18670=DIRECTION('ref_axis',(1.,0.,0.));
#18671=DIRECTION('',(0.,1.,0.));
#18672=DIRECTION('center_axis',(0.,-1.,0.));
#18673=DIRECTION('ref_axis',(0.,0.,-1.));
#18674=DIRECTION('center_axis',(0.,-1.,0.));
#18675=DIRECTION('ref_axis',(1.,0.,0.));
#18676=DIRECTION('center_axis',(0.,-1.,0.));
#18677=DIRECTION('ref_axis',(1.,0.,0.));
#18678=DIRECTION('',(0.,1.,0.));
#18679=DIRECTION('axis',(0.,0.,1.));
#18680=DIRECTION('refdir',(1.,0.,0.));
#18681=DIRECTION('center_axis',(0.,1.,0.));
#18682=DIRECTION('ref_axis',(0.,0.,1.));
#18683=DIRECTION('center_axis',(0.,1.,0.));
#18684=DIRECTION('ref_axis',(1.,0.,0.));
#18685=DIRECTION('',(1.,0.,0.));
#18686=DIRECTION('center_axis',(0.,-1.,0.));
#18687=DIRECTION('ref_axis',(1.,0.,0.));
#18688=DIRECTION('',(-1.,0.,0.));
#18689=DIRECTION('center_axis',(0.,0.,-1.));
#18690=DIRECTION('ref_axis',(-1.,0.,0.));
#18691=DIRECTION('',(0.,-1.,0.));
#18692=DIRECTION('',(0.,1.,0.));
#18693=DIRECTION('',(1.,0.,0.));
#18694=DIRECTION('center_axis',(0.,-1.,0.));
#18695=DIRECTION('ref_axis',(0.,0.,-1.));
#18696=DIRECTION('center_axis',(0.,-1.,0.));
#18697=DIRECTION('ref_axis',(1.,0.,0.));
#18698=DIRECTION('center_axis',(0.,1.,0.));
#18699=DIRECTION('ref_axis',(1.,0.,0.));
#18700=DIRECTION('',(-1.,0.,0.));
#18701=DIRECTION('center_axis',(0.,0.,1.));
#18702=DIRECTION('ref_axis',(1.,0.,0.));
#18703=DIRECTION('',(0.,1.,0.));
#18704=DIRECTION('',(0.,-1.,0.));
#18705=DIRECTION('center_axis',(0.,1.,0.));
#18706=DIRECTION('ref_axis',(0.,0.,1.));
#18707=DIRECTION('center_axis',(0.,-1.,0.));
#18708=DIRECTION('ref_axis',(1.,0.,0.));
#18709=DIRECTION('center_axis',(0.,-1.,0.));
#18710=DIRECTION('ref_axis',(1.,0.,0.));
#18711=DIRECTION('center_axis',(0.,-1.,0.));
#18712=DIRECTION('ref_axis',(1.,0.,0.));
#18713=DIRECTION('center_axis',(0.,-1.,0.));
#18714=DIRECTION('ref_axis',(1.,0.,0.));
#18715=DIRECTION('',(0.,1.,0.));
#18716=DIRECTION('center_axis',(0.,-1.,0.));
#18717=DIRECTION('ref_axis',(0.,0.,-1.));
#18718=DIRECTION('center_axis',(0.,-1.,0.));
#18719=DIRECTION('ref_axis',(1.,0.,0.));
#18720=DIRECTION('center_axis',(0.,-1.,0.));
#18721=DIRECTION('ref_axis',(1.,0.,0.));
#18722=DIRECTION('',(0.,1.,0.));
#18723=DIRECTION('',(0.,0.,1.));
#18724=DIRECTION('',(1.,0.,0.));
#18725=DIRECTION('',(0.,0.,1.));
#18726=DIRECTION('',(1.,0.,0.));
#18727=DIRECTION('axis',(0.,0.,1.));
#18728=DIRECTION('refdir',(1.,0.,0.));
#18729=DIRECTION('center_axis',(0.,1.,0.));
#18730=DIRECTION('ref_axis',(1.,0.,0.));
#18731=DIRECTION('center_axis',(0.,1.,0.));
#18732=DIRECTION('ref_axis',(1.,0.,0.));
#18733=DIRECTION('center_axis',(0.866025403784439,0.,-0.5));
#18734=DIRECTION('ref_axis',(0.5,0.,0.866025403784439));
#18735=DIRECTION('',(0.5,0.,0.866025403784439));
#18736=DIRECTION('',(0.,-1.,0.));
#18737=DIRECTION('',(0.5,0.,0.866025403784439));
#18738=DIRECTION('',(0.,-1.,0.));
#18739=DIRECTION('center_axis',(1.20185167898973E-16,0.,-1.));
#18740=DIRECTION('ref_axis',(1.,0.,1.20185167898973E-16));
#18741=DIRECTION('',(1.,0.,1.20185167898973E-16));
#18742=DIRECTION('',(0.,-1.,0.));
#18743=DIRECTION('',(1.,0.,1.20185167898973E-16));
#18744=DIRECTION('center_axis',(-0.866025403784439,0.,-0.5));
#18745=DIRECTION('ref_axis',(0.5,0.,-0.866025403784439));
#18746=DIRECTION('',(0.5,0.,-0.866025403784439));
#18747=DIRECTION('',(0.,-1.,0.));
#18748=DIRECTION('',(0.5,0.,-0.866025403784439));
#18749=DIRECTION('center_axis',(-0.866025403784439,0.,0.5));
#18750=DIRECTION('ref_axis',(-0.5,0.,-0.866025403784439));
#18751=DIRECTION('',(-0.5,0.,-0.866025403784439));
#18752=DIRECTION('',(0.,-1.,0.));
#18753=DIRECTION('',(-0.5,0.,-0.866025403784439));
#18754=DIRECTION('center_axis',(-2.40370335797945E-16,0.,1.));
#18755=DIRECTION('ref_axis',(-1.,0.,-2.40370335797945E-16));
#18756=DIRECTION('',(-1.,0.,-2.40370335797945E-16));
#18757=DIRECTION('',(0.,-1.,0.));
#18758=DIRECTION('',(-1.,0.,-2.40370335797945E-16));
#18759=DIRECTION('center_axis',(0.866025403784439,0.,0.5));
#18760=DIRECTION('ref_axis',(-0.5,0.,0.866025403784439));
#18761=DIRECTION('',(-0.5,0.,0.866025403784439));
#18762=DIRECTION('',(-0.5,0.,0.866025403784439));
#18763=DIRECTION('center_axis',(0.,-1.,0.));
#18764=DIRECTION('ref_axis',(0.,0.,-1.));
#18765=DIRECTION('center_axis',(0.,1.,0.));
#18766=DIRECTION('ref_axis',(0.,0.,1.));
#18767=DIRECTION('center_axis',(0.,-1.,0.));
#18768=DIRECTION('ref_axis',(1.,0.,0.));
#18769=DIRECTION('center_axis',(0.,-1.,0.));
#18770=DIRECTION('ref_axis',(1.,0.,0.));
#18771=DIRECTION('center_axis',(0.,-1.,0.));
#18772=DIRECTION('ref_axis',(1.,0.,0.));
#18773=DIRECTION('',(0.707106781186548,0.707106781186547,8.65956056235494E-17));
#18774=DIRECTION('center_axis',(0.,-1.,0.));
#18775=DIRECTION('ref_axis',(1.,0.,0.));
#18776=DIRECTION('',(0.,1.,0.));
#18777=DIRECTION('axis',(0.,0.,1.));
#18778=DIRECTION('refdir',(1.,0.,0.));
#18779=DIRECTION('axis',(0.,0.,1.));
#18780=DIRECTION('refdir',(1.,0.,0.));
#18781=DIRECTION('center_axis',(0.,1.,0.));
#18782=DIRECTION('ref_axis',(1.,0.,0.));
#18783=DIRECTION('center_axis',(0.,1.,0.));
#18784=DIRECTION('ref_axis',(1.,0.,0.));
#18785=DIRECTION('',(0.,1.,0.));
#18786=DIRECTION('center_axis',(0.,-1.,0.));
#18787=DIRECTION('ref_axis',(1.,0.,0.));
#18788=DIRECTION('center_axis',(0.,1.,0.));
#18789=DIRECTION('ref_axis',(1.,0.,0.));
#18790=DIRECTION('',(0.,1.,0.));
#18791=DIRECTION('center_axis',(0.,1.,0.));
#18792=DIRECTION('ref_axis',(1.,0.,0.));
#18793=DIRECTION('',(0.,-1.,0.));
#18794=DIRECTION('center_axis',(0.,1.,0.));
#18795=DIRECTION('ref_axis',(1.,0.,0.));
#18796=DIRECTION('center_axis',(0.,1.,0.));
#18797=DIRECTION('ref_axis',(1.,0.,0.));
#18798=DIRECTION('',(0.,-1.,0.));
#18799=DIRECTION('center_axis',(0.,1.,0.));
#18800=DIRECTION('ref_axis',(1.,0.,0.));
#18801=DIRECTION('',(0.,1.,0.));
#18802=DIRECTION('center_axis',(0.,1.,0.));
#18803=DIRECTION('ref_axis',(1.,0.,0.));
#18804=DIRECTION('center_axis',(0.25,0.,-0.968245836551854));
#18805=DIRECTION('ref_axis',(-0.968245836551854,0.,-0.25));
#18806=DIRECTION('',(-0.968245836551854,0.,-0.25));
#18807=DIRECTION('',(0.,-1.,0.));
#18808=DIRECTION('',(-0.968245836551854,0.,-0.25));
#18809=DIRECTION('center_axis',(0.25,0.,-0.968245836551854));
#18810=DIRECTION('ref_axis',(-0.968245836551854,0.,-0.25));
#18811=DIRECTION('',(-0.968245836551854,0.,-0.25));
#18812=DIRECTION('',(0.,1.,0.));
#18813=DIRECTION('',(-0.968245836551854,0.,-0.25));
#18814=DIRECTION('center_axis',(-0.25,0.,0.968245836551854));
#18815=DIRECTION('ref_axis',(0.968245836551854,0.,0.25));
#18816=DIRECTION('',(0.968245836551854,0.,0.25));
#18817=DIRECTION('',(0.,1.,0.));
#18818=DIRECTION('',(0.968245836551854,0.,0.25));
#18819=DIRECTION('center_axis',(0.,1.,0.));
#18820=DIRECTION('ref_axis',(1.,0.,0.));
#18821=DIRECTION('center_axis',(0.,1.,0.));
#18822=DIRECTION('ref_axis',(1.,0.,0.));
#18823=DIRECTION('',(0.,1.,0.));
#18824=DIRECTION('center_axis',(0.,-1.,0.));
#18825=DIRECTION('ref_axis',(1.,0.,0.));
#18826=DIRECTION('center_axis',(0.,1.,0.));
#18827=DIRECTION('ref_axis',(1.,0.,0.));
#18828=DIRECTION('center_axis',(0.,1.,0.));
#18829=DIRECTION('ref_axis',(1.,0.,0.));
#18830=DIRECTION('center_axis',(0.,1.,0.));
#18831=DIRECTION('ref_axis',(1.,0.,0.));
#18832=DIRECTION('center_axis',(0.,1.,0.));
#18833=DIRECTION('ref_axis',(1.,0.,0.));
#18834=DIRECTION('',(0.968245836551854,0.,0.25));
#18835=DIRECTION('center_axis',(0.,1.,0.));
#18836=DIRECTION('ref_axis',(1.,0.,0.));
#18837=DIRECTION('center_axis',(0.,1.,0.));
#18838=DIRECTION('ref_axis',(1.,0.,0.));
#18839=DIRECTION('center_axis',(-0.25,0.,0.968245836551854));
#18840=DIRECTION('ref_axis',(0.968245836551854,0.,0.25));
#18841=DIRECTION('',(0.968245836551854,0.,0.25));
#18842=DIRECTION('',(0.,-1.,0.));
#18843=DIRECTION('center_axis',(0.,1.,0.));
#18844=DIRECTION('ref_axis',(1.,0.,0.));
#18845=DIRECTION('',(0.,1.,0.));
#18846=DIRECTION('center_axis',(0.,-1.,0.));
#18847=DIRECTION('ref_axis',(1.,0.,0.));
#18848=DIRECTION('center_axis',(0.,1.,0.));
#18849=DIRECTION('ref_axis',(-0.968245836551854,0.,-0.250000000000002));
#18850=DIRECTION('center_axis',(0.,1.,0.));
#18851=DIRECTION('ref_axis',(1.,0.,0.));
#18852=DIRECTION('center_axis',(0.,1.,0.));
#18853=DIRECTION('ref_axis',(0.,0.,1.));
#18854=DIRECTION('axis',(0.,0.,1.));
#18855=DIRECTION('refdir',(1.,0.,0.));
#18856=DIRECTION('center_axis',(0.,1.,0.));
#18857=DIRECTION('ref_axis',(1.,0.,0.));
#18858=DIRECTION('center_axis',(0.,-1.,0.));
#18859=DIRECTION('ref_axis',(1.,0.,0.));
#18860=DIRECTION('',(0.,-1.,0.));
#18861=DIRECTION('center_axis',(0.,-1.,0.));
#18862=DIRECTION('ref_axis',(1.,0.,0.));
#18863=DIRECTION('center_axis',(0.,1.,0.));
#18864=DIRECTION('ref_axis',(1.,0.,0.));
#18865=DIRECTION('center_axis',(0.,1.,0.));
#18866=DIRECTION('ref_axis',(1.,0.,0.));
#18867=DIRECTION('',(0.,-1.,0.));
#18868=DIRECTION('center_axis',(0.,1.,0.));
#18869=DIRECTION('ref_axis',(1.,0.,0.));
#18870=DIRECTION('center_axis',(0.,1.,0.));
#18871=DIRECTION('ref_axis',(1.,0.,0.));
#18872=DIRECTION('center_axis',(0.,1.,0.));
#18873=DIRECTION('ref_axis',(1.,0.,0.));
#18874=DIRECTION('axis',(0.,0.,1.));
#18875=DIRECTION('refdir',(1.,0.,0.));
#18876=DIRECTION('center_axis',(0.,1.,0.));
#18877=DIRECTION('ref_axis',(1.,0.,0.));
#18878=DIRECTION('center_axis',(0.,-1.,0.));
#18879=DIRECTION('ref_axis',(1.,0.,0.));
#18880=DIRECTION('',(0.,-1.,0.));
#18881=DIRECTION('center_axis',(0.,-1.,0.));
#18882=DIRECTION('ref_axis',(1.,0.,0.));
#18883=DIRECTION('center_axis',(0.,1.,0.));
#18884=DIRECTION('ref_axis',(1.,0.,0.));
#18885=DIRECTION('center_axis',(0.,1.,0.));
#18886=DIRECTION('ref_axis',(1.,0.,0.));
#18887=DIRECTION('',(0.,-1.,0.));
#18888=DIRECTION('center_axis',(0.,1.,0.));
#18889=DIRECTION('ref_axis',(1.,0.,0.));
#18890=DIRECTION('center_axis',(0.,1.,0.));
#18891=DIRECTION('ref_axis',(1.,0.,0.));
#18892=DIRECTION('center_axis',(0.,1.,0.));
#18893=DIRECTION('ref_axis',(1.,0.,0.));
#18894=DIRECTION('axis',(0.,0.,1.));
#18895=DIRECTION('refdir',(1.,0.,0.));
#18896=DIRECTION('center_axis',(0.,1.,0.));
#18897=DIRECTION('ref_axis',(1.,0.,0.));
#18898=DIRECTION('center_axis',(0.,-1.,0.));
#18899=DIRECTION('ref_axis',(1.,0.,0.));
#18900=DIRECTION('',(0.,-1.,0.));
#18901=DIRECTION('center_axis',(0.,-1.,0.));
#18902=DIRECTION('ref_axis',(1.,0.,0.));
#18903=DIRECTION('center_axis',(0.,1.,0.));
#18904=DIRECTION('ref_axis',(1.,0.,0.));
#18905=DIRECTION('center_axis',(0.,1.,0.));
#18906=DIRECTION('ref_axis',(1.,0.,0.));
#18907=DIRECTION('',(0.,-1.,0.));
#18908=DIRECTION('center_axis',(0.,1.,0.));
#18909=DIRECTION('ref_axis',(1.,0.,0.));
#18910=DIRECTION('center_axis',(0.,1.,0.));
#18911=DIRECTION('ref_axis',(1.,0.,0.));
#18912=DIRECTION('center_axis',(0.,1.,0.));
#18913=DIRECTION('ref_axis',(1.,0.,0.));
#18914=DIRECTION('axis',(0.,0.,1.));
#18915=DIRECTION('refdir',(1.,0.,0.));
#18916=DIRECTION('center_axis',(0.,1.,0.));
#18917=DIRECTION('ref_axis',(1.,0.,0.));
#18918=DIRECTION('center_axis',(0.,1.,0.));
#18919=DIRECTION('ref_axis',(1.,0.,0.));
#18920=DIRECTION('',(0.,1.,0.));
#18921=DIRECTION('center_axis',(0.,-1.,0.));
#18922=DIRECTION('ref_axis',(1.,0.,0.));
#18923=DIRECTION('center_axis',(0.,1.,0.));
#18924=DIRECTION('ref_axis',(1.,0.,0.));
#18925=DIRECTION('',(0.,1.,0.));
#18926=DIRECTION('center_axis',(0.,1.,0.));
#18927=DIRECTION('ref_axis',(1.,0.,0.));
#18928=DIRECTION('',(0.,-1.,0.));
#18929=DIRECTION('center_axis',(0.,1.,0.));
#18930=DIRECTION('ref_axis',(1.,0.,0.));
#18931=DIRECTION('center_axis',(0.,1.,0.));
#18932=DIRECTION('ref_axis',(1.,0.,0.));
#18933=DIRECTION('',(0.,-1.,0.));
#18934=DIRECTION('center_axis',(0.,1.,0.));
#18935=DIRECTION('ref_axis',(1.,0.,0.));
#18936=DIRECTION('',(0.,1.,0.));
#18937=DIRECTION('center_axis',(0.,1.,0.));
#18938=DIRECTION('ref_axis',(1.,0.,0.));
#18939=DIRECTION('center_axis',(0.25,0.,-0.968245836551854));
#18940=DIRECTION('ref_axis',(-0.968245836551854,0.,-0.25));
#18941=DIRECTION('',(-0.968245836551854,0.,-0.25));
#18942=DIRECTION('',(0.,-1.,0.));
#18943=DIRECTION('',(-0.968245836551854,0.,-0.25));
#18944=DIRECTION('center_axis',(0.25,0.,-0.968245836551854));
#18945=DIRECTION('ref_axis',(-0.968245836551854,0.,-0.25));
#18946=DIRECTION('',(-0.968245836551854,0.,-0.25));
#18947=DIRECTION('',(0.,1.,0.));
#18948=DIRECTION('',(-0.968245836551854,0.,-0.25));
#18949=DIRECTION('center_axis',(-0.25,0.,0.968245836551854));
#18950=DIRECTION('ref_axis',(0.968245836551854,0.,0.25));
#18951=DIRECTION('',(0.968245836551854,0.,0.25));
#18952=DIRECTION('',(0.,1.,0.));
#18953=DIRECTION('',(0.968245836551854,0.,0.25));
#18954=DIRECTION('center_axis',(0.,1.,0.));
#18955=DIRECTION('ref_axis',(1.,0.,0.));
#18956=DIRECTION('center_axis',(0.,1.,0.));
#18957=DIRECTION('ref_axis',(1.,0.,0.));
#18958=DIRECTION('',(0.,1.,0.));
#18959=DIRECTION('center_axis',(0.,-1.,0.));
#18960=DIRECTION('ref_axis',(1.,0.,0.));
#18961=DIRECTION('center_axis',(0.,1.,0.));
#18962=DIRECTION('ref_axis',(1.,0.,0.));
#18963=DIRECTION('center_axis',(0.,1.,0.));
#18964=DIRECTION('ref_axis',(1.,0.,0.));
#18965=DIRECTION('center_axis',(0.,1.,0.));
#18966=DIRECTION('ref_axis',(1.,0.,0.));
#18967=DIRECTION('center_axis',(0.,1.,0.));
#18968=DIRECTION('ref_axis',(1.,0.,0.));
#18969=DIRECTION('',(0.968245836551854,0.,0.25));
#18970=DIRECTION('center_axis',(0.,1.,0.));
#18971=DIRECTION('ref_axis',(1.,0.,0.));
#18972=DIRECTION('center_axis',(0.,1.,0.));
#18973=DIRECTION('ref_axis',(1.,0.,0.));
#18974=DIRECTION('center_axis',(-0.25,0.,0.968245836551854));
#18975=DIRECTION('ref_axis',(0.968245836551854,0.,0.25));
#18976=DIRECTION('',(0.968245836551854,0.,0.25));
#18977=DIRECTION('',(0.,-1.,0.));
#18978=DIRECTION('center_axis',(0.,1.,0.));
#18979=DIRECTION('ref_axis',(1.,0.,0.));
#18980=DIRECTION('',(0.,1.,0.));
#18981=DIRECTION('center_axis',(0.,-1.,0.));
#18982=DIRECTION('ref_axis',(1.,0.,0.));
#18983=DIRECTION('center_axis',(0.,1.,0.));
#18984=DIRECTION('ref_axis',(-0.968245836551854,0.,-0.250000000000002));
#18985=DIRECTION('center_axis',(0.,1.,0.));
#18986=DIRECTION('ref_axis',(1.,0.,0.));
#18987=DIRECTION('center_axis',(0.,1.,0.));
#18988=DIRECTION('ref_axis',(0.,0.,1.));
#18989=DIRECTION('axis',(0.,0.,1.));
#18990=DIRECTION('refdir',(1.,0.,0.));
#18991=DIRECTION('center_axis',(0.,1.,0.));
#18992=DIRECTION('ref_axis',(1.,0.,0.));
#18993=DIRECTION('center_axis',(0.,-1.,0.));
#18994=DIRECTION('ref_axis',(1.,0.,0.));
#18995=DIRECTION('',(0.,-1.,0.));
#18996=DIRECTION('center_axis',(0.,-1.,0.));
#18997=DIRECTION('ref_axis',(1.,0.,0.));
#18998=DIRECTION('center_axis',(0.,1.,0.));
#18999=DIRECTION('ref_axis',(1.,0.,0.));
#19000=DIRECTION('center_axis',(0.,1.,0.));
#19001=DIRECTION('ref_axis',(1.,0.,0.));
#19002=DIRECTION('',(0.,-1.,0.));
#19003=DIRECTION('center_axis',(0.,1.,0.));
#19004=DIRECTION('ref_axis',(1.,0.,0.));
#19005=DIRECTION('center_axis',(0.,1.,0.));
#19006=DIRECTION('ref_axis',(1.,0.,0.));
#19007=DIRECTION('center_axis',(0.,1.,0.));
#19008=DIRECTION('ref_axis',(1.,0.,0.));
#19009=DIRECTION('axis',(0.,0.,1.));
#19010=DIRECTION('refdir',(1.,0.,0.));
#19011=DIRECTION('center_axis',(0.,1.,0.));
#19012=DIRECTION('ref_axis',(1.,0.,0.));
#19013=DIRECTION('center_axis',(0.,-1.,0.));
#19014=DIRECTION('ref_axis',(1.,0.,0.));
#19015=DIRECTION('',(0.,-1.,0.));
#19016=DIRECTION('center_axis',(0.,-1.,0.));
#19017=DIRECTION('ref_axis',(1.,0.,0.));
#19018=DIRECTION('center_axis',(0.,1.,0.));
#19019=DIRECTION('ref_axis',(1.,0.,0.));
#19020=DIRECTION('center_axis',(0.,1.,0.));
#19021=DIRECTION('ref_axis',(1.,0.,0.));
#19022=DIRECTION('',(0.,-1.,0.));
#19023=DIRECTION('center_axis',(0.,1.,0.));
#19024=DIRECTION('ref_axis',(1.,0.,0.));
#19025=DIRECTION('center_axis',(0.,1.,0.));
#19026=DIRECTION('ref_axis',(1.,0.,0.));
#19027=DIRECTION('center_axis',(0.,1.,0.));
#19028=DIRECTION('ref_axis',(1.,0.,0.));
#19029=DIRECTION('axis',(0.,0.,1.));
#19030=DIRECTION('refdir',(1.,0.,0.));
#19031=DIRECTION('center_axis',(0.,1.,0.));
#19032=DIRECTION('ref_axis',(1.,0.,0.));
#19033=DIRECTION('center_axis',(0.,-1.,0.));
#19034=DIRECTION('ref_axis',(1.,0.,0.));
#19035=DIRECTION('',(0.,-1.,0.));
#19036=DIRECTION('center_axis',(0.,-1.,0.));
#19037=DIRECTION('ref_axis',(1.,0.,0.));
#19038=DIRECTION('center_axis',(0.,1.,0.));
#19039=DIRECTION('ref_axis',(1.,0.,0.));
#19040=DIRECTION('center_axis',(0.,1.,0.));
#19041=DIRECTION('ref_axis',(1.,0.,0.));
#19042=DIRECTION('',(0.,-1.,0.));
#19043=DIRECTION('center_axis',(0.,1.,0.));
#19044=DIRECTION('ref_axis',(1.,0.,0.));
#19045=DIRECTION('center_axis',(0.,1.,0.));
#19046=DIRECTION('ref_axis',(1.,0.,0.));
#19047=DIRECTION('center_axis',(0.,1.,0.));
#19048=DIRECTION('ref_axis',(1.,0.,0.));
#19049=DIRECTION('axis',(0.,0.,1.));
#19050=DIRECTION('refdir',(1.,0.,0.));
#19051=DIRECTION('center_axis',(0.,1.,0.));
#19052=DIRECTION('ref_axis',(1.,0.,0.));
#19053=DIRECTION('center_axis',(0.,1.,0.));
#19054=DIRECTION('ref_axis',(1.,0.,0.));
#19055=DIRECTION('',(0.,1.,0.));
#19056=DIRECTION('center_axis',(0.,-1.,0.));
#19057=DIRECTION('ref_axis',(1.,0.,0.));
#19058=DIRECTION('center_axis',(0.,1.,0.));
#19059=DIRECTION('ref_axis',(1.,0.,0.));
#19060=DIRECTION('center_axis',(0.,1.,0.));
#19061=DIRECTION('ref_axis',(1.,0.,0.));
#19062=DIRECTION('center_axis',(0.,1.,0.));
#19063=DIRECTION('ref_axis',(1.,0.,0.));
#19064=DIRECTION('',(0.,1.,0.));
#19065=DIRECTION('center_axis',(0.,1.,0.));
#19066=DIRECTION('ref_axis',(1.,0.,0.));
#19067=DIRECTION('center_axis',(0.,1.,0.));
#19068=DIRECTION('ref_axis',(1.,0.,0.));
#19069=DIRECTION('center_axis',(0.,1.,0.));
#19070=DIRECTION('ref_axis',(1.,0.,0.));
#19071=DIRECTION('center_axis',(0.,1.,0.));
#19072=DIRECTION('ref_axis',(1.,0.,0.));
#19073=DIRECTION('',(0.,-1.,0.));
#19074=DIRECTION('center_axis',(0.,1.,0.));
#19075=DIRECTION('ref_axis',(1.,0.,0.));
#19076=DIRECTION('center_axis',(0.,1.,0.));
#19077=DIRECTION('ref_axis',(1.,0.,0.));
#19078=DIRECTION('center_axis',(0.,1.,0.));
#19079=DIRECTION('ref_axis',(1.,0.,0.));
#19080=DIRECTION('axis',(0.,0.,1.));
#19081=DIRECTION('refdir',(1.,0.,0.));
#19082=DIRECTION('center_axis',(0.,1.,0.));
#19083=DIRECTION('ref_axis',(1.,0.,0.));
#19084=DIRECTION('center_axis',(0.,-1.,0.));
#19085=DIRECTION('ref_axis',(1.,0.,0.));
#19086=DIRECTION('',(0.,-1.,0.));
#19087=DIRECTION('center_axis',(0.,-1.,0.));
#19088=DIRECTION('ref_axis',(1.,0.,0.));
#19089=DIRECTION('center_axis',(0.,1.,0.));
#19090=DIRECTION('ref_axis',(1.,0.,0.));
#19091=DIRECTION('center_axis',(0.,1.,0.));
#19092=DIRECTION('ref_axis',(1.,0.,0.));
#19093=DIRECTION('',(0.,-1.,0.));
#19094=DIRECTION('center_axis',(0.,1.,0.));
#19095=DIRECTION('ref_axis',(1.,0.,0.));
#19096=DIRECTION('center_axis',(0.,1.,0.));
#19097=DIRECTION('ref_axis',(1.,0.,0.));
#19098=DIRECTION('center_axis',(0.,1.,0.));
#19099=DIRECTION('ref_axis',(1.,0.,0.));
#19100=DIRECTION('axis',(0.,0.,1.));
#19101=DIRECTION('refdir',(1.,0.,0.));
#19102=DIRECTION('center_axis',(0.,1.,0.));
#19103=DIRECTION('ref_axis',(1.,0.,0.));
#19104=DIRECTION('center_axis',(0.,-1.,0.));
#19105=DIRECTION('ref_axis',(1.,0.,0.));
#19106=DIRECTION('',(0.,-1.,0.));
#19107=DIRECTION('center_axis',(0.,-1.,0.));
#19108=DIRECTION('ref_axis',(1.,0.,0.));
#19109=DIRECTION('center_axis',(0.,1.,0.));
#19110=DIRECTION('ref_axis',(1.,0.,0.));
#19111=DIRECTION('center_axis',(0.,1.,0.));
#19112=DIRECTION('ref_axis',(1.,0.,0.));
#19113=DIRECTION('',(0.,-1.,0.));
#19114=DIRECTION('center_axis',(0.,1.,0.));
#19115=DIRECTION('ref_axis',(1.,0.,0.));
#19116=DIRECTION('center_axis',(0.,1.,0.));
#19117=DIRECTION('ref_axis',(1.,0.,0.));
#19118=DIRECTION('center_axis',(0.,1.,0.));
#19119=DIRECTION('ref_axis',(1.,0.,0.));
#19120=DIRECTION('axis',(0.,0.,1.));
#19121=DIRECTION('refdir',(1.,0.,0.));
#19122=DIRECTION('center_axis',(0.,1.,0.));
#19123=DIRECTION('ref_axis',(1.,0.,0.));
#19124=DIRECTION('center_axis',(0.,-1.,0.));
#19125=DIRECTION('ref_axis',(1.,0.,0.));
#19126=DIRECTION('',(0.,-1.,0.));
#19127=DIRECTION('center_axis',(0.,-1.,0.));
#19128=DIRECTION('ref_axis',(1.,0.,0.));
#19129=DIRECTION('center_axis',(0.,1.,0.));
#19130=DIRECTION('ref_axis',(1.,0.,0.));
#19131=DIRECTION('center_axis',(0.,1.,0.));
#19132=DIRECTION('ref_axis',(1.,0.,0.));
#19133=DIRECTION('',(0.,-1.,0.));
#19134=DIRECTION('center_axis',(0.,1.,0.));
#19135=DIRECTION('ref_axis',(1.,0.,0.));
#19136=DIRECTION('center_axis',(0.,1.,0.));
#19137=DIRECTION('ref_axis',(1.,0.,0.));
#19138=DIRECTION('center_axis',(0.,1.,0.));
#19139=DIRECTION('ref_axis',(1.,0.,0.));
#19140=DIRECTION('axis',(0.,0.,1.));
#19141=DIRECTION('refdir',(1.,0.,0.));
#19142=DIRECTION('center_axis',(0.,1.,0.));
#19143=DIRECTION('ref_axis',(1.,0.,0.));
#19144=DIRECTION('center_axis',(0.,-1.,0.));
#19145=DIRECTION('ref_axis',(1.,0.,0.));
#19146=DIRECTION('',(0.,-1.,0.));
#19147=DIRECTION('center_axis',(0.,-1.,0.));
#19148=DIRECTION('ref_axis',(1.,0.,0.));
#19149=DIRECTION('center_axis',(0.,1.,0.));
#19150=DIRECTION('ref_axis',(1.,0.,0.));
#19151=DIRECTION('center_axis',(0.,1.,0.));
#19152=DIRECTION('ref_axis',(1.,0.,0.));
#19153=DIRECTION('',(0.,-1.,0.));
#19154=DIRECTION('center_axis',(0.,1.,0.));
#19155=DIRECTION('ref_axis',(1.,0.,0.));
#19156=DIRECTION('center_axis',(0.,1.,0.));
#19157=DIRECTION('ref_axis',(1.,0.,0.));
#19158=DIRECTION('center_axis',(0.,1.,0.));
#19159=DIRECTION('ref_axis',(1.,0.,0.));
#19160=DIRECTION('axis',(0.,0.,1.));
#19161=DIRECTION('refdir',(1.,0.,0.));
#19162=DIRECTION('center_axis',(0.,1.,0.));
#19163=DIRECTION('ref_axis',(1.,0.,0.));
#19164=DIRECTION('center_axis',(0.,-1.,0.));
#19165=DIRECTION('ref_axis',(1.,0.,0.));
#19166=DIRECTION('',(0.,-1.,0.));
#19167=DIRECTION('center_axis',(0.,-1.,0.));
#19168=DIRECTION('ref_axis',(1.,0.,0.));
#19169=DIRECTION('center_axis',(0.,1.,0.));
#19170=DIRECTION('ref_axis',(1.,0.,0.));
#19171=DIRECTION('center_axis',(0.,1.,0.));
#19172=DIRECTION('ref_axis',(1.,0.,0.));
#19173=DIRECTION('',(0.,-1.,0.));
#19174=DIRECTION('center_axis',(0.,1.,0.));
#19175=DIRECTION('ref_axis',(1.,0.,0.));
#19176=DIRECTION('center_axis',(0.,1.,0.));
#19177=DIRECTION('ref_axis',(1.,0.,0.));
#19178=DIRECTION('center_axis',(0.,1.,0.));
#19179=DIRECTION('ref_axis',(1.,0.,0.));
#19180=DIRECTION('axis',(0.,0.,1.));
#19181=DIRECTION('refdir',(1.,0.,0.));
#19182=DIRECTION('center_axis',(0.,1.,0.));
#19183=DIRECTION('ref_axis',(1.,0.,0.));
#19184=DIRECTION('center_axis',(0.,-1.,0.));
#19185=DIRECTION('ref_axis',(1.,0.,0.));
#19186=DIRECTION('',(0.,-1.,0.));
#19187=DIRECTION('center_axis',(0.,-1.,0.));
#19188=DIRECTION('ref_axis',(1.,0.,0.));
#19189=DIRECTION('center_axis',(0.,1.,0.));
#19190=DIRECTION('ref_axis',(1.,0.,0.));
#19191=DIRECTION('center_axis',(0.,1.,0.));
#19192=DIRECTION('ref_axis',(1.,0.,0.));
#19193=DIRECTION('',(0.,-1.,0.));
#19194=DIRECTION('center_axis',(0.,1.,0.));
#19195=DIRECTION('ref_axis',(1.,0.,0.));
#19196=DIRECTION('center_axis',(0.,1.,0.));
#19197=DIRECTION('ref_axis',(1.,0.,0.));
#19198=DIRECTION('center_axis',(0.,1.,0.));
#19199=DIRECTION('ref_axis',(1.,0.,0.));
#19200=DIRECTION('axis',(0.,0.,1.));
#19201=DIRECTION('refdir',(1.,0.,0.));
#19202=DIRECTION('center_axis',(0.,1.,0.));
#19203=DIRECTION('ref_axis',(1.,0.,0.));
#19204=DIRECTION('center_axis',(0.,-1.,0.));
#19205=DIRECTION('ref_axis',(1.,0.,0.));
#19206=DIRECTION('',(0.,-1.,0.));
#19207=DIRECTION('center_axis',(0.,-1.,0.));
#19208=DIRECTION('ref_axis',(1.,0.,0.));
#19209=DIRECTION('center_axis',(0.,1.,0.));
#19210=DIRECTION('ref_axis',(1.,0.,0.));
#19211=DIRECTION('center_axis',(0.,1.,0.));
#19212=DIRECTION('ref_axis',(1.,0.,0.));
#19213=DIRECTION('',(0.,-1.,0.));
#19214=DIRECTION('center_axis',(0.,1.,0.));
#19215=DIRECTION('ref_axis',(1.,0.,0.));
#19216=DIRECTION('center_axis',(0.,1.,0.));
#19217=DIRECTION('ref_axis',(1.,0.,0.));
#19218=DIRECTION('center_axis',(0.,1.,0.));
#19219=DIRECTION('ref_axis',(1.,0.,0.));
#19220=DIRECTION('axis',(0.,0.,1.));
#19221=DIRECTION('refdir',(1.,0.,0.));
#19222=DIRECTION('center_axis',(0.,1.,0.));
#19223=DIRECTION('ref_axis',(0.,0.,1.));
#19224=DIRECTION('center_axis',(0.,-1.,0.));
#19225=DIRECTION('ref_axis',(1.,0.,0.));
#19226=DIRECTION('center_axis',(0.,-1.,0.));
#19227=DIRECTION('ref_axis',(1.,0.,0.));
#19228=DIRECTION('center_axis',(0.,-1.,0.));
#19229=DIRECTION('ref_axis',(1.,0.,0.));
#19230=DIRECTION('',(0.707106781186547,0.707106781186548,8.65956056235493E-17));
#19231=DIRECTION('center_axis',(0.,-1.,0.));
#19232=DIRECTION('ref_axis',(1.,0.,0.));
#19233=DIRECTION('center_axis',(0.,-1.,0.));
#19234=DIRECTION('ref_axis',(1.,0.,0.));
#19235=DIRECTION('',(0.,1.,0.));
#19236=DIRECTION('center_axis',(0.,1.,0.));
#19237=DIRECTION('ref_axis',(1.,0.,0.));
#19238=DIRECTION('center_axis',(0.,-1.,0.));
#19239=DIRECTION('ref_axis',(1.,0.,0.));
#19240=DIRECTION('',(-0.707106781186547,0.707106781186548,-8.65956056235493E-17));
#19241=DIRECTION('center_axis',(0.,-1.,0.));
#19242=DIRECTION('ref_axis',(0.,0.,-1.));
#19243=DIRECTION('center_axis',(0.,-1.,0.));
#19244=DIRECTION('ref_axis',(1.,0.,0.));
#19245=DIRECTION('center_axis',(0.,1.,0.));
#19246=DIRECTION('ref_axis',(1.,0.,0.));
#19247=DIRECTION('center_axis',(0.,1.,0.));
#19248=DIRECTION('ref_axis',(1.,0.,0.));
#19249=DIRECTION('',(-0.447213595499958,0.894427190999916,-5.47678698264203E-17));
#19250=DIRECTION('center_axis',(0.,-1.,0.));
#19251=DIRECTION('ref_axis',(1.,0.,0.));
#19252=DIRECTION('center_axis',(0.,1.,0.));
#19253=DIRECTION('ref_axis',(1.,0.,0.));
#19254=DIRECTION('',(0.,1.,0.));
#19255=DIRECTION('center_axis',(0.,1.,0.));
#19256=DIRECTION('ref_axis',(1.,0.,0.));
#19257=DIRECTION('center_axis',(0.,-1.,0.));
#19258=DIRECTION('ref_axis',(1.,0.,0.));
#19259=DIRECTION('',(-0.707106781186547,0.707106781186548,-8.65956056235493E-17));
#19260=DIRECTION('center_axis',(0.,-1.,0.));
#19261=DIRECTION('ref_axis',(0.,0.,-1.));
#19262=DIRECTION('center_axis',(0.866025403784439,0.,-0.5));
#19263=DIRECTION('ref_axis',(0.5,0.,0.866025403784439));
#19264=DIRECTION('',(-0.5,0.,-0.866025403784439));
#19265=DIRECTION('',(0.,-1.,0.));
#19266=DIRECTION('',(0.5,0.,0.866025403784439));
#19267=DIRECTION('',(0.,-1.,0.));
#19268=DIRECTION('center_axis',(1.60246890531964E-16,0.,-1.));
#19269=DIRECTION('ref_axis',(1.,0.,1.60246890531964E-16));
#19270=DIRECTION('',(-1.,0.,-1.60246890531964E-16));
#19271=DIRECTION('',(0.,-1.,0.));
#19272=DIRECTION('',(1.,0.,1.60246890531964E-16));
#19273=DIRECTION('center_axis',(-0.866025403784439,0.,-0.5));
#19274=DIRECTION('ref_axis',(0.5,0.,-0.866025403784439));
#19275=DIRECTION('',(-0.5,0.,0.866025403784439));
#19276=DIRECTION('',(0.,-1.,0.));
#19277=DIRECTION('',(0.5,0.,-0.866025403784439));
#19278=DIRECTION('center_axis',(-0.866025403784439,0.,0.5));
#19279=DIRECTION('ref_axis',(-0.5,0.,-0.866025403784439));
#19280=DIRECTION('',(0.5,0.,0.866025403784439));
#19281=DIRECTION('',(0.,-1.,0.));
#19282=DIRECTION('',(-0.5,0.,-0.866025403784439));
#19283=DIRECTION('center_axis',(-1.60246890531964E-16,0.,1.));
#19284=DIRECTION('ref_axis',(-1.,0.,-1.60246890531964E-16));
#19285=DIRECTION('',(1.,0.,1.60246890531964E-16));
#19286=DIRECTION('',(0.,-1.,0.));
#19287=DIRECTION('',(-1.,0.,-1.60246890531964E-16));
#19288=DIRECTION('center_axis',(0.866025403784439,0.,0.5));
#19289=DIRECTION('ref_axis',(-0.5,0.,0.866025403784439));
#19290=DIRECTION('',(0.5,0.,-0.866025403784439));
#19291=DIRECTION('',(-0.5,0.,0.866025403784439));
#19292=DIRECTION('center_axis',(0.,1.,0.));
#19293=DIRECTION('ref_axis',(1.,0.,0.));
#19294=DIRECTION('center_axis',(0.,-1.,0.));
#19295=DIRECTION('ref_axis',(0.,0.,-1.));
#19296=DIRECTION('',(0.,0.,1.));
#19297=DIRECTION('',(1.,0.,0.));
#19298=DIRECTION('',(0.,0.,1.));
#19299=DIRECTION('',(1.,0.,0.));
#19300=DIRECTION('',(0.,0.,1.));
#19301=DIRECTION('',(1.,0.,0.));
#19302=DIRECTION('',(0.,0.,1.));
#19303=DIRECTION('',(1.,0.,0.));
#19304=DIRECTION('',(0.,0.,1.));
#19305=DIRECTION('',(1.,0.,0.));
#19306=DIRECTION('',(0.,0.,1.));
#19307=DIRECTION('',(1.,0.,0.));
#19308=DIRECTION('',(0.,0.,1.));
#19309=DIRECTION('',(1.,0.,0.));
#19310=DIRECTION('',(0.,0.,1.));
#19311=DIRECTION('',(1.,0.,0.));
#19312=DIRECTION('',(0.,0.,1.));
#19313=DIRECTION('',(1.,0.,0.));
#19314=DIRECTION('',(0.,0.,1.));
#19315=DIRECTION('',(1.,0.,0.));
#19316=DIRECTION('',(0.,0.,1.));
#19317=DIRECTION('',(1.,0.,0.));
#19318=DIRECTION('',(0.,0.,1.));
#19319=DIRECTION('',(1.,0.,0.));
#19320=DIRECTION('',(0.,-1.,2.22044604925031E-16));
#19321=DIRECTION('',(1.,0.,0.));
#19322=DIRECTION('',(0.,-1.,2.22044604925031E-16));
#19323=DIRECTION('',(1.,0.,0.));
#19324=DIRECTION('',(0.,-1.,2.22044604925031E-16));
#19325=DIRECTION('',(1.,0.,0.));
#19326=DIRECTION('',(0.,-1.,2.22044604925031E-16));
#19327=DIRECTION('',(1.,0.,0.));
#19328=DIRECTION('',(0.,-1.,2.22044604925031E-16));
#19329=DIRECTION('',(1.,0.,0.));
#19330=DIRECTION('',(0.,-1.,2.22044604925031E-16));
#19331=DIRECTION('',(1.,0.,0.));
#19332=DIRECTION('',(0.,-1.,2.22044604925031E-16));
#19333=DIRECTION('',(1.,0.,0.));
#19334=DIRECTION('',(0.,-1.,2.22044604925031E-16));
#19335=DIRECTION('',(1.,0.,0.));
#19336=DIRECTION('',(0.,0.,1.));
#19337=DIRECTION('',(-1.,1.22464679914735E-16,0.));
#19338=DIRECTION('',(0.,0.,1.));
#19339=DIRECTION('',(1.,0.,0.));
#19340=DIRECTION('',(0.,0.,1.));
#19341=DIRECTION('',(1.,0.,0.));
#19342=DIRECTION('',(0.,0.,1.));
#19343=DIRECTION('',(1.,0.,0.));
#19344=DIRECTION('',(0.,0.,1.));
#19345=DIRECTION('',(1.,0.,0.));
#19346=DIRECTION('',(0.,0.,1.));
#19347=DIRECTION('',(1.,0.,0.));
#19348=DIRECTION('',(0.,0.,1.));
#19349=DIRECTION('',(1.,0.,0.));
#19350=DIRECTION('',(0.,0.,1.));
#19351=DIRECTION('',(1.,0.,0.));
#19352=DIRECTION('',(0.,0.,1.));
#19353=DIRECTION('',(1.,0.,0.));
#19354=DIRECTION('',(0.,0.,1.));
#19355=DIRECTION('',(1.,0.,0.));
#19356=DIRECTION('',(0.,0.,1.));
#19357=DIRECTION('',(1.,0.,0.));
#19358=DIRECTION('',(0.,0.,1.));
#19359=DIRECTION('',(1.,0.,0.));
#19360=DIRECTION('',(0.,0.,1.));
#19361=DIRECTION('',(1.,0.,0.));
#19362=DIRECTION('',(0.,0.,1.));
#19363=DIRECTION('',(2.22044604925031E-16,-1.,0.));
#19364=DIRECTION('',(0.,0.,1.));
#19365=DIRECTION('',(2.22044604925031E-16,-1.,0.));
#19366=DIRECTION('',(0.,0.,1.));
#19367=DIRECTION('',(2.22044604925031E-16,-1.,0.));
#19368=DIRECTION('',(0.,0.,1.));
#19369=DIRECTION('',(-1.,1.22464679914735E-16,0.));
#19370=DIRECTION('',(0.,0.,1.));
#19371=DIRECTION('',(1.,0.,0.));
#19372=DIRECTION('',(0.,0.,1.));
#19373=DIRECTION('',(1.,0.,0.));
#19374=DIRECTION('',(0.,0.,1.));
#19375=DIRECTION('',(1.,0.,0.));
#19376=DIRECTION('',(0.,0.,1.));
#19377=DIRECTION('',(1.,0.,0.));
#19378=DIRECTION('',(0.,0.,1.));
#19379=DIRECTION('',(1.,0.,0.));
#19380=DIRECTION('',(0.,0.,1.));
#19381=DIRECTION('',(1.,0.,0.));
#19382=DIRECTION('',(0.,0.,1.));
#19383=DIRECTION('',(1.,0.,0.));
#19384=DIRECTION('',(0.,0.,1.));
#19385=DIRECTION('',(1.,0.,0.));
#19386=DIRECTION('',(0.,0.,1.));
#19387=DIRECTION('',(1.,0.,0.));
#19388=DIRECTION('',(0.,0.,1.));
#19389=DIRECTION('',(1.,0.,0.));
#19390=DIRECTION('',(0.,0.,1.));
#19391=DIRECTION('',(1.,0.,0.));
#19392=DIRECTION('',(0.,0.,1.));
#19393=DIRECTION('',(1.,0.,0.));
#19394=DIRECTION('',(0.,0.,1.));
#19395=DIRECTION('',(2.22044604925031E-16,-1.,0.));
#19396=DIRECTION('',(0.,0.,1.));
#19397=DIRECTION('',(2.22044604925031E-16,-1.,0.));
#19398=DIRECTION('',(0.,0.,1.));
#19399=DIRECTION('',(2.22044604925031E-16,-1.,0.));
#19400=DIRECTION('',(0.,0.,1.));
#19401=DIRECTION('',(-1.,1.22464679914735E-16,0.));
#19402=DIRECTION('',(0.,0.,1.));
#19403=DIRECTION('',(1.,0.,0.));
#19404=DIRECTION('',(0.,0.,1.));
#19405=DIRECTION('',(1.,0.,0.));
#19406=DIRECTION('',(0.,0.,1.));
#19407=DIRECTION('',(1.,0.,0.));
#19408=DIRECTION('',(0.,0.,1.));
#19409=DIRECTION('',(1.,0.,0.));
#19410=DIRECTION('',(0.,0.,1.));
#19411=DIRECTION('',(1.,0.,0.));
#19412=DIRECTION('',(0.,0.,1.));
#19413=DIRECTION('',(1.,0.,0.));
#19414=DIRECTION('',(0.,0.,1.));
#19415=DIRECTION('',(1.,0.,0.));
#19416=DIRECTION('',(0.,0.,1.));
#19417=DIRECTION('',(1.,0.,0.));
#19418=DIRECTION('',(0.,0.,1.));
#19419=DIRECTION('',(1.,0.,0.));
#19420=DIRECTION('',(0.,0.,1.));
#19421=DIRECTION('',(1.,0.,0.));
#19422=DIRECTION('',(0.,0.,1.));
#19423=DIRECTION('',(1.,0.,0.));
#19424=DIRECTION('',(0.,0.,1.));
#19425=DIRECTION('',(1.,0.,0.));
#19426=DIRECTION('',(0.,0.,1.));
#19427=DIRECTION('',(1.,0.,0.));
#19428=DIRECTION('',(0.,0.,1.));
#19429=DIRECTION('',(1.,0.,0.));
#19430=DIRECTION('',(0.,0.,1.));
#19431=DIRECTION('',(1.,0.,0.));
#19432=DIRECTION('',(0.,0.,1.));
#19433=DIRECTION('',(1.,0.,0.));
#19434=DIRECTION('',(0.,0.,1.));
#19435=DIRECTION('',(1.,0.,0.));
#19436=DIRECTION('',(0.,0.,1.));
#19437=DIRECTION('',(-1.,1.22464679914735E-16,0.));
#19438=DIRECTION('',(0.,0.,1.));
#19439=DIRECTION('',(1.,0.,0.));
#19440=DIRECTION('axis',(0.,0.,1.));
#19441=DIRECTION('refdir',(1.,0.,0.));
#19442=DIRECTION('axis',(0.,0.,1.));
#19443=DIRECTION('refdir',(1.,0.,0.));
#19444=DIRECTION('center_axis',(0.,1.,0.));
#19445=DIRECTION('ref_axis',(1.,0.,0.));
#19446=DIRECTION('center_axis',(0.,1.,0.));
#19447=DIRECTION('ref_axis',(1.,0.,0.));
#19448=DIRECTION('',(0.,1.,0.));
#19449=DIRECTION('center_axis',(0.,-1.,0.));
#19450=DIRECTION('ref_axis',(1.,0.,0.));
#19451=DIRECTION('center_axis',(0.,1.,0.));
#19452=DIRECTION('ref_axis',(1.,0.,0.));
#19453=DIRECTION('center_axis',(0.,1.,0.));
#19454=DIRECTION('ref_axis',(1.,0.,0.));
#19455=DIRECTION('',(0.,1.,0.));
#19456=DIRECTION('center_axis',(0.,-1.,0.));
#19457=DIRECTION('ref_axis',(1.,0.,0.));
#19458=DIRECTION('center_axis',(0.,1.,0.));
#19459=DIRECTION('ref_axis',(1.,0.,0.));
#19460=DIRECTION('center_axis',(0.,1.,0.));
#19461=DIRECTION('ref_axis',(1.,0.,0.));
#19462=DIRECTION('',(0.,1.,0.));
#19463=DIRECTION('center_axis',(0.,-1.,0.));
#19464=DIRECTION('ref_axis',(1.,0.,0.));
#19465=DIRECTION('center_axis',(0.,1.,0.));
#19466=DIRECTION('ref_axis',(1.,0.,0.));
#19467=DIRECTION('center_axis',(0.,1.,0.));
#19468=DIRECTION('ref_axis',(1.,0.,0.));
#19469=DIRECTION('',(0.,1.,0.));
#19470=DIRECTION('center_axis',(0.,-1.,0.));
#19471=DIRECTION('ref_axis',(1.,0.,0.));
#19472=DIRECTION('center_axis',(0.,1.,0.));
#19473=DIRECTION('ref_axis',(1.,0.,0.));
#19474=DIRECTION('center_axis',(0.,1.,0.));
#19475=DIRECTION('ref_axis',(1.,0.,0.));
#19476=DIRECTION('',(0.,1.,0.));
#19477=DIRECTION('center_axis',(0.,-1.,0.));
#19478=DIRECTION('ref_axis',(1.,0.,0.));
#19479=DIRECTION('center_axis',(0.,1.,0.));
#19480=DIRECTION('ref_axis',(1.,0.,0.));
#19481=DIRECTION('',(0.,-1.,0.));
#19482=DIRECTION('center_axis',(0.,1.,0.));
#19483=DIRECTION('ref_axis',(1.,0.,0.));
#19484=DIRECTION('',(0.,1.,0.));
#19485=DIRECTION('center_axis',(0.,1.,0.));
#19486=DIRECTION('ref_axis',(1.,0.,0.));
#19487=DIRECTION('center_axis',(0.,1.,0.));
#19488=DIRECTION('ref_axis',(1.,0.,0.));
#19489=DIRECTION('',(0.,1.,0.));
#19490=DIRECTION('center_axis',(0.,1.,0.));
#19491=DIRECTION('ref_axis',(1.,0.,0.));
#19492=DIRECTION('',(0.,-1.,0.));
#19493=DIRECTION('center_axis',(0.,1.,0.));
#19494=DIRECTION('ref_axis',(1.,0.,0.));
#19495=DIRECTION('center_axis',(0.25,0.,0.968245836551854));
#19496=DIRECTION('ref_axis',(0.968245836551854,0.,-0.25));
#19497=DIRECTION('',(0.968245836551854,0.,-0.25));
#19498=DIRECTION('',(0.,1.,0.));
#19499=DIRECTION('',(0.968245836551854,0.,-0.25));
#19500=DIRECTION('center_axis',(0.,1.,0.));
#19501=DIRECTION('ref_axis',(0.,0.,1.));
#19502=DIRECTION('center_axis',(0.,1.,0.));
#19503=DIRECTION('ref_axis',(1.,0.,0.));
#19504=DIRECTION('',(-0.968245836551854,0.,0.25));
#19505=DIRECTION('',(-0.968245836551854,0.,0.25));
#19506=DIRECTION('center_axis',(0.,1.,0.));
#19507=DIRECTION('ref_axis',(1.,0.,0.));
#19508=DIRECTION('',(0.968245836551854,0.,-0.25));
#19509=DIRECTION('center_axis',(0.,-1.,0.));
#19510=DIRECTION('ref_axis',(1.,0.,0.));
#19511=DIRECTION('center_axis',(0.,-1.,0.));
#19512=DIRECTION('ref_axis',(1.,0.,0.));
#19513=DIRECTION('center_axis',(-0.25,0.,-0.968245836551854));
#19514=DIRECTION('ref_axis',(-0.968245836551854,0.,0.25));
#19515=DIRECTION('',(0.,-1.,0.));
#19516=DIRECTION('',(-0.968245836551854,0.,0.25));
#19517=DIRECTION('center_axis',(0.,1.,0.));
#19518=DIRECTION('ref_axis',(1.,0.,0.));
#19519=DIRECTION('center_axis',(0.,1.,0.));
#19520=DIRECTION('ref_axis',(1.,0.,0.));
#19521=DIRECTION('',(0.,1.,0.));
#19522=DIRECTION('center_axis',(0.,1.,0.));
#19523=DIRECTION('ref_axis',(-0.968245836551855,0.,0.249999999999998));
#19524=DIRECTION('',(0.,1.,0.));
#19525=DIRECTION('center_axis',(0.,1.,0.));
#19526=DIRECTION('ref_axis',(1.,0.,0.));
#19527=DIRECTION('',(0.,-1.,0.));
#19528=DIRECTION('center_axis',(-0.25,0.,-0.968245836551854));
#19529=DIRECTION('ref_axis',(-0.968245836551854,0.,0.25));
#19530=DIRECTION('',(-0.968245836551854,0.,0.25));
#19531=DIRECTION('center_axis',(0.,1.,0.));
#19532=DIRECTION('ref_axis',(1.,0.,0.));
#19533=DIRECTION('center_axis',(0.,1.,0.));
#19534=DIRECTION('ref_axis',(1.,0.,0.));
#19535=DIRECTION('',(0.,1.,0.));
#19536=DIRECTION('center_axis',(0.,1.,0.));
#19537=DIRECTION('ref_axis',(1.,0.,0.));
#19538=DIRECTION('center_axis',(0.,1.,0.));
#19539=DIRECTION('ref_axis',(1.,0.,0.));
#19540=DIRECTION('center_axis',(0.25,0.,0.968245836551854));
#19541=DIRECTION('ref_axis',(0.968245836551854,0.,-0.25));
#19542=DIRECTION('',(0.968245836551854,0.,-0.25));
#19543=DIRECTION('center_axis',(0.,1.,0.));
#19544=DIRECTION('ref_axis',(1.,0.,0.));
#19545=DIRECTION('axis',(0.,0.,1.));
#19546=DIRECTION('refdir',(1.,0.,0.));
#19547=DIRECTION('center_axis',(0.,1.,0.));
#19548=DIRECTION('ref_axis',(1.,0.,0.));
#19549=DIRECTION('center_axis',(0.,-1.,0.));
#19550=DIRECTION('ref_axis',(1.,0.,0.));
#19551=DIRECTION('',(0.,-1.,0.));
#19552=DIRECTION('center_axis',(0.,-1.,0.));
#19553=DIRECTION('ref_axis',(1.,0.,0.));
#19554=DIRECTION('center_axis',(0.,1.,0.));
#19555=DIRECTION('ref_axis',(1.,0.,0.));
#19556=DIRECTION('center_axis',(0.,1.,0.));
#19557=DIRECTION('ref_axis',(1.,0.,0.));
#19558=DIRECTION('',(0.,-1.,0.));
#19559=DIRECTION('center_axis',(0.,1.,0.));
#19560=DIRECTION('ref_axis',(1.,0.,0.));
#19561=DIRECTION('center_axis',(0.,1.,0.));
#19562=DIRECTION('ref_axis',(1.,0.,0.));
#19563=DIRECTION('center_axis',(0.,1.,0.));
#19564=DIRECTION('ref_axis',(1.,0.,0.));
#19565=DIRECTION('axis',(0.,0.,1.));
#19566=DIRECTION('refdir',(1.,0.,0.));
#19567=DIRECTION('center_axis',(0.,1.,0.));
#19568=DIRECTION('ref_axis',(1.,0.,0.));
#19569=DIRECTION('center_axis',(0.,-1.,0.));
#19570=DIRECTION('ref_axis',(1.,0.,0.));
#19571=DIRECTION('',(0.,-1.,0.));
#19572=DIRECTION('center_axis',(0.,-1.,0.));
#19573=DIRECTION('ref_axis',(1.,0.,0.));
#19574=DIRECTION('center_axis',(0.,1.,0.));
#19575=DIRECTION('ref_axis',(1.,0.,0.));
#19576=DIRECTION('center_axis',(0.,1.,0.));
#19577=DIRECTION('ref_axis',(1.,0.,0.));
#19578=DIRECTION('',(0.,-1.,0.));
#19579=DIRECTION('center_axis',(0.,1.,0.));
#19580=DIRECTION('ref_axis',(1.,0.,0.));
#19581=DIRECTION('center_axis',(0.,1.,0.));
#19582=DIRECTION('ref_axis',(1.,0.,0.));
#19583=DIRECTION('center_axis',(0.,1.,0.));
#19584=DIRECTION('ref_axis',(1.,0.,0.));
#19585=DIRECTION('axis',(0.,0.,1.));
#19586=DIRECTION('refdir',(1.,0.,0.));
#19587=DIRECTION('center_axis',(0.,1.,0.));
#19588=DIRECTION('ref_axis',(1.,0.,0.));
#19589=DIRECTION('center_axis',(0.,1.,0.));
#19590=DIRECTION('ref_axis',(1.,0.,0.));
#19591=DIRECTION('',(0.,1.,0.));
#19592=DIRECTION('center_axis',(0.,-1.,0.));
#19593=DIRECTION('ref_axis',(1.,0.,0.));
#19594=DIRECTION('center_axis',(0.,1.,0.));
#19595=DIRECTION('ref_axis',(1.,0.,0.));
#19596=DIRECTION('center_axis',(0.,1.,0.));
#19597=DIRECTION('ref_axis',(1.,0.,0.));
#19598=DIRECTION('',(0.,1.,0.));
#19599=DIRECTION('center_axis',(0.,-1.,0.));
#19600=DIRECTION('ref_axis',(1.,0.,0.));
#19601=DIRECTION('center_axis',(0.,1.,0.));
#19602=DIRECTION('ref_axis',(1.,0.,0.));
#19603=DIRECTION('center_axis',(0.,1.,0.));
#19604=DIRECTION('ref_axis',(1.,0.,0.));
#19605=DIRECTION('',(0.,1.,0.));
#19606=DIRECTION('center_axis',(0.,-1.,0.));
#19607=DIRECTION('ref_axis',(1.,0.,0.));
#19608=DIRECTION('center_axis',(0.,1.,0.));
#19609=DIRECTION('ref_axis',(1.,0.,0.));
#19610=DIRECTION('center_axis',(0.,1.,0.));
#19611=DIRECTION('ref_axis',(1.,0.,0.));
#19612=DIRECTION('',(0.,1.,0.));
#19613=DIRECTION('center_axis',(0.,-1.,0.));
#19614=DIRECTION('ref_axis',(1.,0.,0.));
#19615=DIRECTION('center_axis',(0.,1.,0.));
#19616=DIRECTION('ref_axis',(1.,0.,0.));
#19617=DIRECTION('center_axis',(0.,-1.,0.));
#19618=DIRECTION('ref_axis',(1.,0.,0.));
#19619=DIRECTION('',(0.,-1.,0.));
#19620=DIRECTION('center_axis',(0.,-1.,0.));
#19621=DIRECTION('ref_axis',(1.,0.,0.));
#19622=DIRECTION('center_axis',(0.,1.,0.));
#19623=DIRECTION('ref_axis',(1.,0.,0.));
#19624=DIRECTION('center_axis',(0.,1.,0.));
#19625=DIRECTION('ref_axis',(1.,0.,0.));
#19626=DIRECTION('',(0.,-1.,0.));
#19627=DIRECTION('center_axis',(0.,1.,0.));
#19628=DIRECTION('ref_axis',(1.,0.,0.));
#19629=DIRECTION('center_axis',(0.,1.,0.));
#19630=DIRECTION('ref_axis',(1.,0.,0.));
#19631=DIRECTION('center_axis',(0.,1.,0.));
#19632=DIRECTION('ref_axis',(1.,0.,0.));
#19633=DIRECTION('axis',(0.,0.,1.));
#19634=DIRECTION('refdir',(1.,0.,0.));
#19635=DIRECTION('center_axis',(0.,1.,0.));
#19636=DIRECTION('ref_axis',(1.,0.,0.));
#19637=DIRECTION('center_axis',(0.,1.,0.));
#19638=DIRECTION('ref_axis',(1.,0.,0.));
#19639=DIRECTION('center_axis',(0.,1.,0.));
#19640=DIRECTION('ref_axis',(1.,0.,0.));
#19641=DIRECTION('center_axis',(0.,1.,0.));
#19642=DIRECTION('ref_axis',(1.,0.,0.));
#19643=DIRECTION('',(0.,-1.,0.));
#19644=DIRECTION('center_axis',(0.,1.,0.));
#19645=DIRECTION('ref_axis',(1.,0.,0.));
#19646=DIRECTION('center_axis',(0.,1.,0.));
#19647=DIRECTION('ref_axis',(1.,0.,0.));
#19648=DIRECTION('center_axis',(0.,1.,0.));
#19649=DIRECTION('ref_axis',(1.,0.,0.));
#19650=DIRECTION('center_axis',(0.,1.,0.));
#19651=DIRECTION('ref_axis',(1.,0.,0.));
#19652=DIRECTION('',(0.,-1.,0.));
#19653=DIRECTION('center_axis',(0.,1.,0.));
#19654=DIRECTION('ref_axis',(1.,0.,0.));
#19655=DIRECTION('axis',(0.,0.,1.));
#19656=DIRECTION('refdir',(1.,0.,0.));
#19657=DIRECTION('center_axis',(0.,1.,0.));
#19658=DIRECTION('ref_axis',(1.,0.,0.));
#19659=DIRECTION('center_axis',(0.,1.,0.));
#19660=DIRECTION('ref_axis',(1.,0.,0.));
#19661=DIRECTION('center_axis',(0.,1.,0.));
#19662=DIRECTION('ref_axis',(1.,0.,0.));
#19663=DIRECTION('center_axis',(0.,1.,0.));
#19664=DIRECTION('ref_axis',(1.,0.,0.));
#19665=DIRECTION('',(0.,-1.,0.));
#19666=DIRECTION('center_axis',(0.,1.,0.));
#19667=DIRECTION('ref_axis',(1.,0.,0.));
#19668=DIRECTION('center_axis',(0.,1.,0.));
#19669=DIRECTION('ref_axis',(1.,0.,0.));
#19670=DIRECTION('center_axis',(0.,1.,0.));
#19671=DIRECTION('ref_axis',(1.,0.,0.));
#19672=DIRECTION('center_axis',(0.,1.,0.));
#19673=DIRECTION('ref_axis',(1.,0.,0.));
#19674=DIRECTION('',(0.,-1.,0.));
#19675=DIRECTION('center_axis',(0.,1.,0.));
#19676=DIRECTION('ref_axis',(1.,0.,0.));
#19677=DIRECTION('axis',(0.,0.,1.));
#19678=DIRECTION('refdir',(1.,0.,0.));
#19679=DIRECTION('center_axis',(0.,1.,0.));
#19680=DIRECTION('ref_axis',(1.,0.,0.));
#19681=DIRECTION('center_axis',(0.,1.,0.));
#19682=DIRECTION('ref_axis',(1.,0.,0.));
#19683=DIRECTION('center_axis',(0.,1.,0.));
#19684=DIRECTION('ref_axis',(1.,0.,0.));
#19685=DIRECTION('center_axis',(0.,1.,0.));
#19686=DIRECTION('ref_axis',(1.,0.,0.));
#19687=DIRECTION('',(0.,-1.,0.));
#19688=DIRECTION('center_axis',(0.,1.,0.));
#19689=DIRECTION('ref_axis',(1.,0.,0.));
#19690=DIRECTION('center_axis',(0.,1.,0.));
#19691=DIRECTION('ref_axis',(1.,0.,0.));
#19692=DIRECTION('center_axis',(0.,1.,0.));
#19693=DIRECTION('ref_axis',(1.,0.,0.));
#19694=DIRECTION('center_axis',(0.,1.,0.));
#19695=DIRECTION('ref_axis',(1.,0.,0.));
#19696=DIRECTION('',(0.,-1.,0.));
#19697=DIRECTION('center_axis',(0.,1.,0.));
#19698=DIRECTION('ref_axis',(1.,0.,0.));
#19699=DIRECTION('axis',(0.,0.,1.));
#19700=DIRECTION('refdir',(1.,0.,0.));
#19701=DIRECTION('center_axis',(0.,1.,0.));
#19702=DIRECTION('ref_axis',(1.,0.,0.));
#19703=DIRECTION('center_axis',(0.,1.,0.));
#19704=DIRECTION('ref_axis',(1.,0.,0.));
#19705=DIRECTION('center_axis',(0.,1.,0.));
#19706=DIRECTION('ref_axis',(1.,0.,0.));
#19707=DIRECTION('center_axis',(0.,1.,0.));
#19708=DIRECTION('ref_axis',(1.,0.,0.));
#19709=DIRECTION('',(0.,-1.,0.));
#19710=DIRECTION('center_axis',(0.,1.,0.));
#19711=DIRECTION('ref_axis',(1.,0.,0.));
#19712=DIRECTION('center_axis',(0.,1.,0.));
#19713=DIRECTION('ref_axis',(1.,0.,0.));
#19714=DIRECTION('center_axis',(0.,1.,0.));
#19715=DIRECTION('ref_axis',(1.,0.,0.));
#19716=DIRECTION('center_axis',(0.,1.,0.));
#19717=DIRECTION('ref_axis',(1.,0.,0.));
#19718=DIRECTION('',(0.,-1.,0.));
#19719=DIRECTION('center_axis',(0.,1.,0.));
#19720=DIRECTION('ref_axis',(1.,0.,0.));
#19721=DIRECTION('axis',(0.,0.,1.));
#19722=DIRECTION('refdir',(1.,0.,0.));
#19723=DIRECTION('center_axis',(0.,1.,0.));
#19724=DIRECTION('ref_axis',(1.,0.,0.));
#19725=DIRECTION('center_axis',(0.,1.,0.));
#19726=DIRECTION('ref_axis',(1.,0.,0.));
#19727=DIRECTION('',(0.,1.,0.));
#19728=DIRECTION('center_axis',(0.,-1.,0.));
#19729=DIRECTION('ref_axis',(1.,0.,0.));
#19730=DIRECTION('center_axis',(0.,1.,0.));
#19731=DIRECTION('ref_axis',(1.,0.,0.));
#19732=DIRECTION('center_axis',(0.,1.,0.));
#19733=DIRECTION('ref_axis',(1.,0.,0.));
#19734=DIRECTION('',(0.,1.,0.));
#19735=DIRECTION('center_axis',(0.,-1.,0.));
#19736=DIRECTION('ref_axis',(1.,0.,0.));
#19737=DIRECTION('center_axis',(0.,1.,0.));
#19738=DIRECTION('ref_axis',(1.,0.,0.));
#19739=DIRECTION('center_axis',(0.,1.,0.));
#19740=DIRECTION('ref_axis',(1.,0.,0.));
#19741=DIRECTION('',(0.,1.,0.));
#19742=DIRECTION('center_axis',(0.,-1.,0.));
#19743=DIRECTION('ref_axis',(1.,0.,0.));
#19744=DIRECTION('center_axis',(0.,1.,0.));
#19745=DIRECTION('ref_axis',(1.,0.,0.));
#19746=DIRECTION('center_axis',(0.,1.,0.));
#19747=DIRECTION('ref_axis',(1.,0.,0.));
#19748=DIRECTION('',(0.,1.,0.));
#19749=DIRECTION('center_axis',(0.,-1.,0.));
#19750=DIRECTION('ref_axis',(1.,0.,0.));
#19751=DIRECTION('center_axis',(0.,1.,0.));
#19752=DIRECTION('ref_axis',(1.,0.,0.));
#19753=DIRECTION('center_axis',(0.,-1.,0.));
#19754=DIRECTION('ref_axis',(1.,0.,0.));
#19755=DIRECTION('',(0.,-1.,0.));
#19756=DIRECTION('center_axis',(0.,-1.,0.));
#19757=DIRECTION('ref_axis',(1.,0.,0.));
#19758=DIRECTION('center_axis',(0.,1.,0.));
#19759=DIRECTION('ref_axis',(1.,0.,0.));
#19760=DIRECTION('center_axis',(0.,1.,0.));
#19761=DIRECTION('ref_axis',(1.,0.,0.));
#19762=DIRECTION('',(0.,-1.,0.));
#19763=DIRECTION('center_axis',(0.,1.,0.));
#19764=DIRECTION('ref_axis',(1.,0.,0.));
#19765=DIRECTION('center_axis',(0.,1.,0.));
#19766=DIRECTION('ref_axis',(1.,0.,0.));
#19767=DIRECTION('center_axis',(0.,1.,0.));
#19768=DIRECTION('ref_axis',(1.,0.,0.));
#19769=DIRECTION('axis',(0.,0.,1.));
#19770=DIRECTION('refdir',(1.,0.,0.));
#19771=DIRECTION('center_axis',(0.,1.,0.));
#19772=DIRECTION('ref_axis',(1.,0.,0.));
#19773=DIRECTION('center_axis',(0.,1.,0.));
#19774=DIRECTION('ref_axis',(1.,0.,0.));
#19775=DIRECTION('center_axis',(0.,1.,0.));
#19776=DIRECTION('ref_axis',(1.,0.,0.));
#19777=DIRECTION('center_axis',(0.,1.,0.));
#19778=DIRECTION('ref_axis',(1.,0.,0.));
#19779=DIRECTION('center_axis',(0.,1.,0.));
#19780=DIRECTION('ref_axis',(1.,0.,0.));
#19781=DIRECTION('',(0.,-1.,0.));
#19782=DIRECTION('center_axis',(0.,1.,0.));
#19783=DIRECTION('ref_axis',(1.,0.,0.));
#19784=DIRECTION('center_axis',(0.,1.,0.));
#19785=DIRECTION('ref_axis',(1.,0.,0.));
#19786=DIRECTION('',(0.,-1.,0.));
#19787=DIRECTION('center_axis',(0.,1.,0.));
#19788=DIRECTION('ref_axis',(1.,0.,0.));
#19789=DIRECTION('center_axis',(0.,1.,0.));
#19790=DIRECTION('ref_axis',(1.,0.,0.));
#19791=DIRECTION('axis',(0.,0.,1.));
#19792=DIRECTION('refdir',(1.,0.,0.));
#19793=DIRECTION('center_axis',(0.,1.,0.));
#19794=DIRECTION('ref_axis',(1.,0.,0.));
#19795=DIRECTION('center_axis',(0.,1.,0.));
#19796=DIRECTION('ref_axis',(1.,0.,0.));
#19797=DIRECTION('center_axis',(0.,1.,0.));
#19798=DIRECTION('ref_axis',(1.,0.,0.));
#19799=DIRECTION('center_axis',(0.,1.,0.));
#19800=DIRECTION('ref_axis',(1.,0.,0.));
#19801=DIRECTION('center_axis',(0.,1.,0.));
#19802=DIRECTION('ref_axis',(1.,0.,0.));
#19803=DIRECTION('',(0.,-1.,0.));
#19804=DIRECTION('center_axis',(0.,1.,0.));
#19805=DIRECTION('ref_axis',(1.,0.,0.));
#19806=DIRECTION('center_axis',(0.,1.,0.));
#19807=DIRECTION('ref_axis',(1.,0.,0.));
#19808=DIRECTION('',(0.,-1.,0.));
#19809=DIRECTION('center_axis',(0.,1.,0.));
#19810=DIRECTION('ref_axis',(1.,0.,0.));
#19811=DIRECTION('center_axis',(0.,1.,0.));
#19812=DIRECTION('ref_axis',(1.,0.,0.));
#19813=DIRECTION('axis',(0.,0.,1.));
#19814=DIRECTION('refdir',(1.,0.,0.));
#19815=DIRECTION('center_axis',(0.,1.,0.));
#19816=DIRECTION('ref_axis',(1.,0.,0.));
#19817=DIRECTION('center_axis',(0.,1.,0.));
#19818=DIRECTION('ref_axis',(1.,0.,0.));
#19819=DIRECTION('center_axis',(0.,1.,0.));
#19820=DIRECTION('ref_axis',(1.,0.,0.));
#19821=DIRECTION('center_axis',(0.,1.,0.));
#19822=DIRECTION('ref_axis',(1.,0.,0.));
#19823=DIRECTION('center_axis',(0.,1.,0.));
#19824=DIRECTION('ref_axis',(1.,0.,0.));
#19825=DIRECTION('',(0.,-1.,0.));
#19826=DIRECTION('center_axis',(0.,1.,0.));
#19827=DIRECTION('ref_axis',(1.,0.,0.));
#19828=DIRECTION('center_axis',(0.,1.,0.));
#19829=DIRECTION('ref_axis',(1.,0.,0.));
#19830=DIRECTION('',(0.,-1.,0.));
#19831=DIRECTION('center_axis',(0.,1.,0.));
#19832=DIRECTION('ref_axis',(1.,0.,0.));
#19833=DIRECTION('center_axis',(0.,1.,0.));
#19834=DIRECTION('ref_axis',(1.,0.,0.));
#19835=DIRECTION('axis',(0.,0.,1.));
#19836=DIRECTION('refdir',(1.,0.,0.));
#19837=DIRECTION('center_axis',(0.,1.,0.));
#19838=DIRECTION('ref_axis',(1.,0.,0.));
#19839=DIRECTION('center_axis',(0.,1.,0.));
#19840=DIRECTION('ref_axis',(1.,0.,0.));
#19841=DIRECTION('center_axis',(0.,1.,0.));
#19842=DIRECTION('ref_axis',(1.,0.,0.));
#19843=DIRECTION('center_axis',(0.,1.,0.));
#19844=DIRECTION('ref_axis',(1.,0.,0.));
#19845=DIRECTION('center_axis',(0.,1.,0.));
#19846=DIRECTION('ref_axis',(1.,0.,0.));
#19847=DIRECTION('',(0.,-1.,0.));
#19848=DIRECTION('center_axis',(0.,1.,0.));
#19849=DIRECTION('ref_axis',(1.,0.,0.));
#19850=DIRECTION('center_axis',(0.,1.,0.));
#19851=DIRECTION('ref_axis',(1.,0.,0.));
#19852=DIRECTION('',(0.,-1.,0.));
#19853=DIRECTION('center_axis',(0.,1.,0.));
#19854=DIRECTION('ref_axis',(1.,0.,0.));
#19855=DIRECTION('center_axis',(0.,1.,0.));
#19856=DIRECTION('ref_axis',(1.,0.,0.));
#19857=DIRECTION('axis',(0.,0.,1.));
#19858=DIRECTION('refdir',(1.,0.,0.));
#19859=DIRECTION('center_axis',(0.,1.,0.));
#19860=DIRECTION('ref_axis',(1.,0.,0.));
#19861=DIRECTION('center_axis',(0.,1.,0.));
#19862=DIRECTION('ref_axis',(1.,0.,0.));
#19863=DIRECTION('',(0.,1.,0.));
#19864=DIRECTION('center_axis',(0.,-1.,0.));
#19865=DIRECTION('ref_axis',(1.,0.,0.));
#19866=DIRECTION('center_axis',(0.,1.,0.));
#19867=DIRECTION('ref_axis',(1.,0.,0.));
#19868=DIRECTION('center_axis',(0.,1.,0.));
#19869=DIRECTION('ref_axis',(1.,0.,0.));
#19870=DIRECTION('',(0.,1.,0.));
#19871=DIRECTION('center_axis',(0.,-1.,0.));
#19872=DIRECTION('ref_axis',(1.,0.,0.));
#19873=DIRECTION('center_axis',(0.,1.,0.));
#19874=DIRECTION('ref_axis',(1.,0.,0.));
#19875=DIRECTION('center_axis',(0.,1.,0.));
#19876=DIRECTION('ref_axis',(1.,0.,0.));
#19877=DIRECTION('',(0.,1.,0.));
#19878=DIRECTION('center_axis',(0.,-1.,0.));
#19879=DIRECTION('ref_axis',(1.,0.,0.));
#19880=DIRECTION('center_axis',(0.,1.,0.));
#19881=DIRECTION('ref_axis',(1.,0.,0.));
#19882=DIRECTION('center_axis',(0.,1.,0.));
#19883=DIRECTION('ref_axis',(1.,0.,0.));
#19884=DIRECTION('',(0.,1.,0.));
#19885=DIRECTION('center_axis',(0.,-1.,0.));
#19886=DIRECTION('ref_axis',(1.,0.,0.));
#19887=DIRECTION('center_axis',(0.,1.,0.));
#19888=DIRECTION('ref_axis',(1.,0.,0.));
#19889=DIRECTION('center_axis',(0.,1.,0.));
#19890=DIRECTION('ref_axis',(1.,0.,0.));
#19891=DIRECTION('',(0.,1.,0.));
#19892=DIRECTION('center_axis',(0.,-1.,0.));
#19893=DIRECTION('ref_axis',(1.,0.,0.));
#19894=DIRECTION('center_axis',(0.,1.,0.));
#19895=DIRECTION('ref_axis',(1.,0.,0.));
#19896=DIRECTION('',(0.,-1.,0.));
#19897=DIRECTION('center_axis',(0.,1.,0.));
#19898=DIRECTION('ref_axis',(1.,0.,0.));
#19899=DIRECTION('',(0.,1.,0.));
#19900=DIRECTION('center_axis',(0.,1.,0.));
#19901=DIRECTION('ref_axis',(1.,0.,0.));
#19902=DIRECTION('center_axis',(0.,1.,0.));
#19903=DIRECTION('ref_axis',(1.,0.,0.));
#19904=DIRECTION('',(0.,1.,0.));
#19905=DIRECTION('center_axis',(0.,1.,0.));
#19906=DIRECTION('ref_axis',(1.,0.,0.));
#19907=DIRECTION('',(0.,-1.,0.));
#19908=DIRECTION('center_axis',(0.,1.,0.));
#19909=DIRECTION('ref_axis',(1.,0.,0.));
#19910=DIRECTION('center_axis',(0.25,0.,0.968245836551854));
#19911=DIRECTION('ref_axis',(0.968245836551854,0.,-0.25));
#19912=DIRECTION('',(0.968245836551854,0.,-0.25));
#19913=DIRECTION('',(0.,1.,0.));
#19914=DIRECTION('',(0.968245836551854,0.,-0.25));
#19915=DIRECTION('center_axis',(0.,1.,0.));
#19916=DIRECTION('ref_axis',(0.,0.,1.));
#19917=DIRECTION('center_axis',(0.,1.,0.));
#19918=DIRECTION('ref_axis',(1.,0.,0.));
#19919=DIRECTION('',(-0.968245836551854,0.,0.25));
#19920=DIRECTION('',(-0.968245836551854,0.,0.25));
#19921=DIRECTION('center_axis',(0.,1.,0.));
#19922=DIRECTION('ref_axis',(1.,0.,0.));
#19923=DIRECTION('',(0.968245836551854,0.,-0.25));
#19924=DIRECTION('center_axis',(0.,-1.,0.));
#19925=DIRECTION('ref_axis',(1.,0.,0.));
#19926=DIRECTION('center_axis',(0.,-1.,0.));
#19927=DIRECTION('ref_axis',(1.,0.,0.));
#19928=DIRECTION('center_axis',(-0.25,0.,-0.968245836551854));
#19929=DIRECTION('ref_axis',(-0.968245836551854,0.,0.25));
#19930=DIRECTION('',(0.,-1.,0.));
#19931=DIRECTION('',(-0.968245836551854,0.,0.25));
#19932=DIRECTION('center_axis',(0.,1.,0.));
#19933=DIRECTION('ref_axis',(1.,0.,0.));
#19934=DIRECTION('center_axis',(0.,1.,0.));
#19935=DIRECTION('ref_axis',(1.,0.,0.));
#19936=DIRECTION('',(0.,1.,0.));
#19937=DIRECTION('center_axis',(0.,1.,0.));
#19938=DIRECTION('ref_axis',(-0.968245836551855,0.,0.249999999999998));
#19939=DIRECTION('',(0.,1.,0.));
#19940=DIRECTION('center_axis',(0.,1.,0.));
#19941=DIRECTION('ref_axis',(1.,0.,0.));
#19942=DIRECTION('',(0.,-1.,0.));
#19943=DIRECTION('center_axis',(-0.25,0.,-0.968245836551854));
#19944=DIRECTION('ref_axis',(-0.968245836551854,0.,0.25));
#19945=DIRECTION('',(-0.968245836551854,0.,0.25));
#19946=DIRECTION('center_axis',(0.,1.,0.));
#19947=DIRECTION('ref_axis',(1.,0.,0.));
#19948=DIRECTION('center_axis',(0.,1.,0.));
#19949=DIRECTION('ref_axis',(1.,0.,0.));
#19950=DIRECTION('',(0.,1.,0.));
#19951=DIRECTION('center_axis',(0.,1.,0.));
#19952=DIRECTION('ref_axis',(1.,0.,0.));
#19953=DIRECTION('center_axis',(0.,1.,0.));
#19954=DIRECTION('ref_axis',(1.,0.,0.));
#19955=DIRECTION('center_axis',(0.25,0.,0.968245836551854));
#19956=DIRECTION('ref_axis',(0.968245836551854,0.,-0.25));
#19957=DIRECTION('',(0.968245836551854,0.,-0.25));
#19958=DIRECTION('center_axis',(0.,1.,0.));
#19959=DIRECTION('ref_axis',(1.,0.,0.));
#19960=DIRECTION('axis',(0.,0.,1.));
#19961=DIRECTION('refdir',(1.,0.,0.));
#19962=DIRECTION('center_axis',(0.,1.,0.));
#19963=DIRECTION('ref_axis',(1.,0.,0.));
#19964=DIRECTION('center_axis',(0.,-1.,0.));
#19965=DIRECTION('ref_axis',(1.,0.,0.));
#19966=DIRECTION('',(0.,-1.,0.));
#19967=DIRECTION('center_axis',(0.,-1.,0.));
#19968=DIRECTION('ref_axis',(1.,0.,0.));
#19969=DIRECTION('center_axis',(0.,1.,0.));
#19970=DIRECTION('ref_axis',(1.,0.,0.));
#19971=DIRECTION('center_axis',(0.,1.,0.));
#19972=DIRECTION('ref_axis',(1.,0.,0.));
#19973=DIRECTION('',(0.,-1.,0.));
#19974=DIRECTION('center_axis',(0.,1.,0.));
#19975=DIRECTION('ref_axis',(1.,0.,0.));
#19976=DIRECTION('center_axis',(0.,1.,0.));
#19977=DIRECTION('ref_axis',(1.,0.,0.));
#19978=DIRECTION('center_axis',(0.,1.,0.));
#19979=DIRECTION('ref_axis',(1.,0.,0.));
#19980=DIRECTION('axis',(0.,0.,1.));
#19981=DIRECTION('refdir',(1.,0.,0.));
#19982=DIRECTION('center_axis',(0.,1.,0.));
#19983=DIRECTION('ref_axis',(1.,0.,0.));
#19984=DIRECTION('center_axis',(0.,-1.,0.));
#19985=DIRECTION('ref_axis',(1.,0.,0.));
#19986=DIRECTION('',(0.,-1.,0.));
#19987=DIRECTION('center_axis',(0.,-1.,0.));
#19988=DIRECTION('ref_axis',(1.,0.,0.));
#19989=DIRECTION('center_axis',(0.,1.,0.));
#19990=DIRECTION('ref_axis',(1.,0.,0.));
#19991=DIRECTION('center_axis',(0.,1.,0.));
#19992=DIRECTION('ref_axis',(1.,0.,0.));
#19993=DIRECTION('',(0.,-1.,0.));
#19994=DIRECTION('center_axis',(0.,1.,0.));
#19995=DIRECTION('ref_axis',(1.,0.,0.));
#19996=DIRECTION('center_axis',(0.,1.,0.));
#19997=DIRECTION('ref_axis',(1.,0.,0.));
#19998=DIRECTION('center_axis',(0.,1.,0.));
#19999=DIRECTION('ref_axis',(1.,0.,0.));
#20000=DIRECTION('axis',(0.,0.,1.));
#20001=DIRECTION('refdir',(1.,0.,0.));
#20002=DIRECTION('center_axis',(0.,1.,0.));
#20003=DIRECTION('ref_axis',(1.,0.,0.));
#20004=DIRECTION('center_axis',(0.,1.,0.));
#20005=DIRECTION('ref_axis',(1.,0.,0.));
#20006=DIRECTION('',(0.,1.,0.));
#20007=DIRECTION('center_axis',(0.,-1.,0.));
#20008=DIRECTION('ref_axis',(1.,0.,0.));
#20009=DIRECTION('center_axis',(0.,1.,0.));
#20010=DIRECTION('ref_axis',(1.,0.,0.));
#20011=DIRECTION('center_axis',(0.,1.,0.));
#20012=DIRECTION('ref_axis',(1.,0.,0.));
#20013=DIRECTION('',(0.,1.,0.));
#20014=DIRECTION('center_axis',(0.,-1.,0.));
#20015=DIRECTION('ref_axis',(1.,0.,0.));
#20016=DIRECTION('center_axis',(0.,1.,0.));
#20017=DIRECTION('ref_axis',(1.,0.,0.));
#20018=DIRECTION('center_axis',(0.,1.,0.));
#20019=DIRECTION('ref_axis',(1.,0.,0.));
#20020=DIRECTION('',(0.,1.,0.));
#20021=DIRECTION('center_axis',(0.,-1.,0.));
#20022=DIRECTION('ref_axis',(1.,0.,0.));
#20023=DIRECTION('center_axis',(0.,1.,0.));
#20024=DIRECTION('ref_axis',(1.,0.,0.));
#20025=DIRECTION('center_axis',(0.,1.,0.));
#20026=DIRECTION('ref_axis',(1.,0.,0.));
#20027=DIRECTION('',(0.,1.,0.));
#20028=DIRECTION('center_axis',(0.,-1.,0.));
#20029=DIRECTION('ref_axis',(1.,0.,0.));
#20030=DIRECTION('center_axis',(0.,1.,0.));
#20031=DIRECTION('ref_axis',(1.,0.,0.));
#20032=DIRECTION('center_axis',(0.,-1.,0.));
#20033=DIRECTION('ref_axis',(1.,0.,0.));
#20034=DIRECTION('',(0.,-1.,0.));
#20035=DIRECTION('center_axis',(0.,-1.,0.));
#20036=DIRECTION('ref_axis',(1.,0.,0.));
#20037=DIRECTION('center_axis',(0.,1.,0.));
#20038=DIRECTION('ref_axis',(1.,0.,0.));
#20039=DIRECTION('center_axis',(0.,1.,0.));
#20040=DIRECTION('ref_axis',(1.,0.,0.));
#20041=DIRECTION('',(0.,-1.,0.));
#20042=DIRECTION('center_axis',(0.,1.,0.));
#20043=DIRECTION('ref_axis',(1.,0.,0.));
#20044=DIRECTION('center_axis',(0.,1.,0.));
#20045=DIRECTION('ref_axis',(1.,0.,0.));
#20046=DIRECTION('center_axis',(0.,1.,0.));
#20047=DIRECTION('ref_axis',(1.,0.,0.));
#20048=DIRECTION('axis',(0.,0.,1.));
#20049=DIRECTION('refdir',(1.,0.,0.));
#20050=DIRECTION('center_axis',(0.,1.,0.));
#20051=DIRECTION('ref_axis',(1.,0.,0.));
#20052=DIRECTION('center_axis',(0.,1.,0.));
#20053=DIRECTION('ref_axis',(1.,0.,0.));
#20054=DIRECTION('center_axis',(0.,1.,0.));
#20055=DIRECTION('ref_axis',(1.,0.,0.));
#20056=DIRECTION('center_axis',(0.,1.,0.));
#20057=DIRECTION('ref_axis',(1.,0.,0.));
#20058=DIRECTION('',(0.,-1.,0.));
#20059=DIRECTION('center_axis',(0.,1.,0.));
#20060=DIRECTION('ref_axis',(1.,0.,0.));
#20061=DIRECTION('center_axis',(0.,1.,0.));
#20062=DIRECTION('ref_axis',(1.,0.,0.));
#20063=DIRECTION('center_axis',(0.,1.,0.));
#20064=DIRECTION('ref_axis',(1.,0.,0.));
#20065=DIRECTION('center_axis',(0.,1.,0.));
#20066=DIRECTION('ref_axis',(1.,0.,0.));
#20067=DIRECTION('',(0.,-1.,0.));
#20068=DIRECTION('center_axis',(0.,1.,0.));
#20069=DIRECTION('ref_axis',(1.,0.,0.));
#20070=DIRECTION('axis',(0.,0.,1.));
#20071=DIRECTION('refdir',(1.,0.,0.));
#20072=DIRECTION('center_axis',(0.,1.,0.));
#20073=DIRECTION('ref_axis',(1.,0.,0.));
#20074=DIRECTION('center_axis',(0.,1.,0.));
#20075=DIRECTION('ref_axis',(1.,0.,0.));
#20076=DIRECTION('center_axis',(0.,1.,0.));
#20077=DIRECTION('ref_axis',(1.,0.,0.));
#20078=DIRECTION('center_axis',(0.,1.,0.));
#20079=DIRECTION('ref_axis',(1.,0.,0.));
#20080=DIRECTION('',(0.,-1.,0.));
#20081=DIRECTION('center_axis',(0.,1.,0.));
#20082=DIRECTION('ref_axis',(1.,0.,0.));
#20083=DIRECTION('center_axis',(0.,1.,0.));
#20084=DIRECTION('ref_axis',(1.,0.,0.));
#20085=DIRECTION('center_axis',(0.,1.,0.));
#20086=DIRECTION('ref_axis',(1.,0.,0.));
#20087=DIRECTION('center_axis',(0.,1.,0.));
#20088=DIRECTION('ref_axis',(1.,0.,0.));
#20089=DIRECTION('',(0.,-1.,0.));
#20090=DIRECTION('center_axis',(0.,1.,0.));
#20091=DIRECTION('ref_axis',(1.,0.,0.));
#20092=DIRECTION('axis',(0.,0.,1.));
#20093=DIRECTION('refdir',(1.,0.,0.));
#20094=DIRECTION('center_axis',(0.,1.,0.));
#20095=DIRECTION('ref_axis',(1.,0.,0.));
#20096=DIRECTION('center_axis',(0.,1.,0.));
#20097=DIRECTION('ref_axis',(1.,0.,0.));
#20098=DIRECTION('center_axis',(0.,1.,0.));
#20099=DIRECTION('ref_axis',(1.,0.,0.));
#20100=DIRECTION('center_axis',(0.,1.,0.));
#20101=DIRECTION('ref_axis',(1.,0.,0.));
#20102=DIRECTION('',(0.,-1.,0.));
#20103=DIRECTION('center_axis',(0.,1.,0.));
#20104=DIRECTION('ref_axis',(1.,0.,0.));
#20105=DIRECTION('center_axis',(0.,1.,0.));
#20106=DIRECTION('ref_axis',(1.,0.,0.));
#20107=DIRECTION('center_axis',(0.,1.,0.));
#20108=DIRECTION('ref_axis',(1.,0.,0.));
#20109=DIRECTION('center_axis',(0.,1.,0.));
#20110=DIRECTION('ref_axis',(1.,0.,0.));
#20111=DIRECTION('',(0.,-1.,0.));
#20112=DIRECTION('center_axis',(0.,1.,0.));
#20113=DIRECTION('ref_axis',(1.,0.,0.));
#20114=DIRECTION('axis',(0.,0.,1.));
#20115=DIRECTION('refdir',(1.,0.,0.));
#20116=DIRECTION('center_axis',(0.,1.,0.));
#20117=DIRECTION('ref_axis',(1.,0.,0.));
#20118=DIRECTION('center_axis',(0.,1.,0.));
#20119=DIRECTION('ref_axis',(1.,0.,0.));
#20120=DIRECTION('center_axis',(0.,1.,0.));
#20121=DIRECTION('ref_axis',(1.,0.,0.));
#20122=DIRECTION('center_axis',(0.,1.,0.));
#20123=DIRECTION('ref_axis',(1.,0.,0.));
#20124=DIRECTION('',(0.,-1.,0.));
#20125=DIRECTION('center_axis',(0.,1.,0.));
#20126=DIRECTION('ref_axis',(1.,0.,0.));
#20127=DIRECTION('center_axis',(0.,1.,0.));
#20128=DIRECTION('ref_axis',(1.,0.,0.));
#20129=DIRECTION('center_axis',(0.,1.,0.));
#20130=DIRECTION('ref_axis',(1.,0.,0.));
#20131=DIRECTION('center_axis',(0.,1.,0.));
#20132=DIRECTION('ref_axis',(1.,0.,0.));
#20133=DIRECTION('',(0.,-1.,0.));
#20134=DIRECTION('center_axis',(0.,1.,0.));
#20135=DIRECTION('ref_axis',(1.,0.,0.));
#20136=DIRECTION('axis',(0.,0.,1.));
#20137=DIRECTION('refdir',(1.,0.,0.));
#20138=DIRECTION('center_axis',(0.,1.,0.));
#20139=DIRECTION('ref_axis',(1.,0.,0.));
#20140=DIRECTION('center_axis',(0.,1.,0.));
#20141=DIRECTION('ref_axis',(1.,0.,0.));
#20142=DIRECTION('',(0.,1.,0.));
#20143=DIRECTION('center_axis',(0.,-1.,0.));
#20144=DIRECTION('ref_axis',(1.,0.,0.));
#20145=DIRECTION('center_axis',(0.,1.,0.));
#20146=DIRECTION('ref_axis',(1.,0.,0.));
#20147=DIRECTION('center_axis',(0.,1.,0.));
#20148=DIRECTION('ref_axis',(1.,0.,0.));
#20149=DIRECTION('',(0.,1.,0.));
#20150=DIRECTION('center_axis',(0.,-1.,0.));
#20151=DIRECTION('ref_axis',(1.,0.,0.));
#20152=DIRECTION('center_axis',(0.,1.,0.));
#20153=DIRECTION('ref_axis',(1.,0.,0.));
#20154=DIRECTION('center_axis',(0.,1.,0.));
#20155=DIRECTION('ref_axis',(1.,0.,0.));
#20156=DIRECTION('',(0.,1.,0.));
#20157=DIRECTION('center_axis',(0.,-1.,0.));
#20158=DIRECTION('ref_axis',(1.,0.,0.));
#20159=DIRECTION('center_axis',(0.,1.,0.));
#20160=DIRECTION('ref_axis',(1.,0.,0.));
#20161=DIRECTION('center_axis',(0.,1.,0.));
#20162=DIRECTION('ref_axis',(1.,0.,0.));
#20163=DIRECTION('',(0.,1.,0.));
#20164=DIRECTION('center_axis',(0.,-1.,0.));
#20165=DIRECTION('ref_axis',(1.,0.,0.));
#20166=DIRECTION('center_axis',(0.,1.,0.));
#20167=DIRECTION('ref_axis',(1.,0.,0.));
#20168=DIRECTION('center_axis',(0.,-1.,0.));
#20169=DIRECTION('ref_axis',(1.,0.,0.));
#20170=DIRECTION('',(0.,-1.,0.));
#20171=DIRECTION('center_axis',(0.,-1.,0.));
#20172=DIRECTION('ref_axis',(1.,0.,0.));
#20173=DIRECTION('center_axis',(0.,1.,0.));
#20174=DIRECTION('ref_axis',(1.,0.,0.));
#20175=DIRECTION('center_axis',(0.,1.,0.));
#20176=DIRECTION('ref_axis',(1.,0.,0.));
#20177=DIRECTION('',(0.,-1.,0.));
#20178=DIRECTION('center_axis',(0.,1.,0.));
#20179=DIRECTION('ref_axis',(1.,0.,0.));
#20180=DIRECTION('center_axis',(0.,1.,0.));
#20181=DIRECTION('ref_axis',(1.,0.,0.));
#20182=DIRECTION('center_axis',(0.,1.,0.));
#20183=DIRECTION('ref_axis',(1.,0.,0.));
#20184=DIRECTION('axis',(0.,0.,1.));
#20185=DIRECTION('refdir',(1.,0.,0.));
#20186=DIRECTION('center_axis',(0.,1.,0.));
#20187=DIRECTION('ref_axis',(1.,0.,0.));
#20188=DIRECTION('center_axis',(0.,1.,0.));
#20189=DIRECTION('ref_axis',(1.,0.,0.));
#20190=DIRECTION('center_axis',(0.,1.,0.));
#20191=DIRECTION('ref_axis',(1.,0.,0.));
#20192=DIRECTION('center_axis',(0.,1.,0.));
#20193=DIRECTION('ref_axis',(1.,0.,0.));
#20194=DIRECTION('center_axis',(0.,1.,0.));
#20195=DIRECTION('ref_axis',(1.,0.,0.));
#20196=DIRECTION('',(0.,-1.,0.));
#20197=DIRECTION('center_axis',(0.,1.,0.));
#20198=DIRECTION('ref_axis',(1.,0.,0.));
#20199=DIRECTION('center_axis',(0.,1.,0.));
#20200=DIRECTION('ref_axis',(1.,0.,0.));
#20201=DIRECTION('',(0.,-1.,0.));
#20202=DIRECTION('center_axis',(0.,1.,0.));
#20203=DIRECTION('ref_axis',(1.,0.,0.));
#20204=DIRECTION('center_axis',(0.,1.,0.));
#20205=DIRECTION('ref_axis',(1.,0.,0.));
#20206=DIRECTION('axis',(0.,0.,1.));
#20207=DIRECTION('refdir',(1.,0.,0.));
#20208=DIRECTION('center_axis',(0.,1.,0.));
#20209=DIRECTION('ref_axis',(1.,0.,0.));
#20210=DIRECTION('center_axis',(0.,1.,0.));
#20211=DIRECTION('ref_axis',(1.,0.,0.));
#20212=DIRECTION('center_axis',(0.,1.,0.));
#20213=DIRECTION('ref_axis',(1.,0.,0.));
#20214=DIRECTION('center_axis',(0.,1.,0.));
#20215=DIRECTION('ref_axis',(1.,0.,0.));
#20216=DIRECTION('center_axis',(0.,1.,0.));
#20217=DIRECTION('ref_axis',(1.,0.,0.));
#20218=DIRECTION('',(0.,-1.,0.));
#20219=DIRECTION('center_axis',(0.,1.,0.));
#20220=DIRECTION('ref_axis',(1.,0.,0.));
#20221=DIRECTION('center_axis',(0.,1.,0.));
#20222=DIRECTION('ref_axis',(1.,0.,0.));
#20223=DIRECTION('',(0.,-1.,0.));
#20224=DIRECTION('center_axis',(0.,1.,0.));
#20225=DIRECTION('ref_axis',(1.,0.,0.));
#20226=DIRECTION('center_axis',(0.,1.,0.));
#20227=DIRECTION('ref_axis',(1.,0.,0.));
#20228=DIRECTION('axis',(0.,0.,1.));
#20229=DIRECTION('refdir',(1.,0.,0.));
#20230=DIRECTION('center_axis',(0.,1.,0.));
#20231=DIRECTION('ref_axis',(1.,0.,0.));
#20232=DIRECTION('center_axis',(0.,1.,0.));
#20233=DIRECTION('ref_axis',(1.,0.,0.));
#20234=DIRECTION('center_axis',(0.,1.,0.));
#20235=DIRECTION('ref_axis',(1.,0.,0.));
#20236=DIRECTION('center_axis',(0.,1.,0.));
#20237=DIRECTION('ref_axis',(1.,0.,0.));
#20238=DIRECTION('center_axis',(0.,1.,0.));
#20239=DIRECTION('ref_axis',(1.,0.,0.));
#20240=DIRECTION('',(0.,-1.,0.));
#20241=DIRECTION('center_axis',(0.,1.,0.));
#20242=DIRECTION('ref_axis',(1.,0.,0.));
#20243=DIRECTION('center_axis',(0.,1.,0.));
#20244=DIRECTION('ref_axis',(1.,0.,0.));
#20245=DIRECTION('',(0.,-1.,0.));
#20246=DIRECTION('center_axis',(0.,1.,0.));
#20247=DIRECTION('ref_axis',(1.,0.,0.));
#20248=DIRECTION('center_axis',(0.,1.,0.));
#20249=DIRECTION('ref_axis',(1.,0.,0.));
#20250=DIRECTION('axis',(0.,0.,1.));
#20251=DIRECTION('refdir',(1.,0.,0.));
#20252=DIRECTION('center_axis',(0.,1.,0.));
#20253=DIRECTION('ref_axis',(1.,0.,0.));
#20254=DIRECTION('center_axis',(0.,1.,0.));
#20255=DIRECTION('ref_axis',(1.,0.,0.));
#20256=DIRECTION('center_axis',(0.,1.,0.));
#20257=DIRECTION('ref_axis',(1.,0.,0.));
#20258=DIRECTION('center_axis',(0.,1.,0.));
#20259=DIRECTION('ref_axis',(1.,0.,0.));
#20260=DIRECTION('center_axis',(0.,1.,0.));
#20261=DIRECTION('ref_axis',(1.,0.,0.));
#20262=DIRECTION('',(0.,-1.,0.));
#20263=DIRECTION('center_axis',(0.,1.,0.));
#20264=DIRECTION('ref_axis',(1.,0.,0.));
#20265=DIRECTION('center_axis',(0.,1.,0.));
#20266=DIRECTION('ref_axis',(1.,0.,0.));
#20267=DIRECTION('',(0.,-1.,0.));
#20268=DIRECTION('center_axis',(0.,1.,0.));
#20269=DIRECTION('ref_axis',(1.,0.,0.));
#20270=DIRECTION('center_axis',(0.,1.,0.));
#20271=DIRECTION('ref_axis',(1.,0.,0.));
#20272=DIRECTION('axis',(0.,0.,1.));
#20273=DIRECTION('refdir',(1.,0.,0.));
#20274=DIRECTION('axis',(0.,0.,1.));
#20275=DIRECTION('refdir',(1.,0.,0.));
#20276=DIRECTION('center_axis',(0.,-1.,0.));
#20277=DIRECTION('ref_axis',(0.,0.,-1.));
#20278=DIRECTION('center_axis',(0.,-1.,0.));
#20279=DIRECTION('ref_axis',(1.,0.,0.));
#20280=DIRECTION('center_axis',(0.,-1.,0.));
#20281=DIRECTION('ref_axis',(1.,0.,0.));
#20282=DIRECTION('center_axis',(1.,0.,1.22464679914735E-16));
#20283=DIRECTION('ref_axis',(-1.22464679914735E-16,0.,1.));
#20284=DIRECTION('center_axis',(0.,1.,0.));
#20285=DIRECTION('ref_axis',(1.,0.,0.));
#20286=DIRECTION('center_axis',(0.,1.,0.));
#20287=DIRECTION('ref_axis',(1.,0.,0.));
#20288=DIRECTION('center_axis',(0.,-1.,0.));
#20289=DIRECTION('ref_axis',(1.,0.,0.));
#20290=DIRECTION('',(0.,1.,0.));
#20291=DIRECTION('center_axis',(0.,-1.,0.));
#20292=DIRECTION('ref_axis',(1.,0.,0.));
#20293=DIRECTION('center_axis',(0.,-1.,0.));
#20294=DIRECTION('ref_axis',(1.,0.,0.));
#20295=DIRECTION('center_axis',(0.,-1.,0.));
#20296=DIRECTION('ref_axis',(1.,0.,0.));
#20297=DIRECTION('',(0.,1.,0.));
#20298=DIRECTION('center_axis',(0.,-1.,0.));
#20299=DIRECTION('ref_axis',(1.,0.,0.));
#20300=DIRECTION('center_axis',(0.,1.,0.));
#20301=DIRECTION('ref_axis',(1.,0.,0.));
#20302=DIRECTION('',(-0.707106781186548,0.707106781186547,-8.65956056235493E-17));
#20303=DIRECTION('center_axis',(0.,-1.,0.));
#20304=DIRECTION('ref_axis',(1.,0.,0.));
#20305=DIRECTION('center_axis',(0.,1.,0.));
#20306=DIRECTION('ref_axis',(0.,0.,1.));
#20307=DIRECTION('center_axis',(0.,-1.,0.));
#20308=DIRECTION('ref_axis',(1.,0.,0.));
#20309=DIRECTION('center_axis',(0.,-1.,0.));
#20310=DIRECTION('ref_axis',(1.,0.,0.));
#20311=DIRECTION('',(0.,1.,0.));
#20312=DIRECTION('center_axis',(0.,-1.,0.));
#20313=DIRECTION('ref_axis',(0.,0.,-1.));
#20314=DIRECTION('center_axis',(0.,-1.,0.));
#20315=DIRECTION('ref_axis',(1.,0.,0.));
#20316=DIRECTION('center_axis',(0.,-1.,0.));
#20317=DIRECTION('ref_axis',(1.,0.,0.));
#20318=DIRECTION('',(0.707106781186548,0.707106781186547,8.65956056235493E-17));
#20319=DIRECTION('axis',(0.,0.,1.));
#20320=DIRECTION('refdir',(1.,0.,0.));
#20321=DIRECTION('center_axis',(0.,-1.,0.));
#20322=DIRECTION('ref_axis',(0.,0.,-1.));
#20323=DIRECTION('center_axis',(0.,-1.,0.));
#20324=DIRECTION('ref_axis',(1.,0.,0.));
#20325=DIRECTION('center_axis',(0.,-1.,0.));
#20326=DIRECTION('ref_axis',(1.,0.,0.));
#20327=DIRECTION('center_axis',(1.,0.,1.22464679914735E-16));
#20328=DIRECTION('ref_axis',(-1.22464679914735E-16,0.,1.));
#20329=DIRECTION('center_axis',(0.,1.,0.));
#20330=DIRECTION('ref_axis',(1.,0.,0.));
#20331=DIRECTION('center_axis',(0.,1.,0.));
#20332=DIRECTION('ref_axis',(1.,0.,0.));
#20333=DIRECTION('center_axis',(0.,-1.,0.));
#20334=DIRECTION('ref_axis',(1.,0.,0.));
#20335=DIRECTION('center_axis',(0.,-1.,0.));
#20336=DIRECTION('ref_axis',(1.,0.,0.));
#20337=DIRECTION('',(0.,1.,0.));
#20338=DIRECTION('center_axis',(0.,1.,0.));
#20339=DIRECTION('ref_axis',(0.,0.,1.));
#20340=DIRECTION('center_axis',(0.,-1.,0.));
#20341=DIRECTION('ref_axis',(1.,0.,0.));
#20342=DIRECTION('center_axis',(0.,-1.,0.));
#20343=DIRECTION('ref_axis',(1.,0.,0.));
#20344=DIRECTION('center_axis',(0.,-1.,0.));
#20345=DIRECTION('ref_axis',(1.,0.,0.));
#20346=DIRECTION('center_axis',(0.,-1.,0.));
#20347=DIRECTION('ref_axis',(1.,0.,0.));
#20348=DIRECTION('',(0.707106781186548,0.707106781186547,8.65956056235494E-17));
#20349=DIRECTION('center_axis',(0.,-1.,0.));
#20350=DIRECTION('ref_axis',(1.,0.,0.));
#20351=DIRECTION('center_axis',(0.,-1.,0.));
#20352=DIRECTION('ref_axis',(1.,0.,0.));
#20353=DIRECTION('',(0.,1.,0.));
#20354=DIRECTION('center_axis',(0.,1.,0.));
#20355=DIRECTION('ref_axis',(1.,0.,0.));
#20356=DIRECTION('center_axis',(0.,-1.,0.));
#20357=DIRECTION('ref_axis',(1.,0.,0.));
#20358=DIRECTION('',(-0.707106781186548,0.707106781186547,-8.65956056235494E-17));
#20359=DIRECTION('center_axis',(0.,-1.,0.));
#20360=DIRECTION('ref_axis',(0.,0.,-1.));
#20361=DIRECTION('center_axis',(0.,-1.,0.));
#20362=DIRECTION('ref_axis',(1.,0.,0.));
#20363=DIRECTION('',(0.,1.,0.));
#20364=DIRECTION('axis',(0.,0.,1.));
#20365=DIRECTION('refdir',(1.,0.,0.));
#20366=DIRECTION('center_axis',(0.,0.,1.));
#20367=DIRECTION('ref_axis',(1.,0.,0.));
#20368=DIRECTION('center_axis',(1.22464679914735E-16,-1.,0.));
#20369=DIRECTION('ref_axis',(-1.,-1.22464679914735E-16,0.));
#20370=DIRECTION('center_axis',(0.78183148246803,0.,0.623489801858733));
#20371=DIRECTION('ref_axis',(0.623489801858734,0.,-0.78183148246803));
#20372=DIRECTION('center_axis',(7.63554790147315E-17,-1.,-9.57467422477103E-17));
#20373=DIRECTION('ref_axis',(-0.623489801858734,-1.22464679914735E-16,0.78183148246803));
#20374=DIRECTION('center_axis',(0.974927912181824,0.,-0.222520933956314));
#20375=DIRECTION('ref_axis',(-0.222520933956314,0.,-0.974927912181824));
#20376=DIRECTION('center_axis',(-2.7250954951288E-17,-1.,-1.19394234705288E-16));
#20377=DIRECTION('ref_axis',(0.222520933956314,-1.22464679914735E-16,0.974927912181824));
#20378=DIRECTION('center_axis',(0.433883739117558,0.,-0.900968867902419));
#20379=DIRECTION('ref_axis',(-0.900968867902419,0.,-0.433883739117558));
#20380=DIRECTION('center_axis',(-1.10336864020811E-16,-1.,-5.31354332312403E-17));
#20381=DIRECTION('ref_axis',(0.900968867902419,-1.22464679914735E-16,0.433883739117558));
#20382=DIRECTION('center_axis',(-0.433883739117558,0.,-0.900968867902419));
#20383=DIRECTION('ref_axis',(-0.900968867902419,0.,0.433883739117558));
#20384=DIRECTION('center_axis',(-1.10336864020811E-16,-1.,5.31354332312403E-17));
#20385=DIRECTION('ref_axis',(0.900968867902419,-1.22464679914735E-16,-0.433883739117558));
#20386=DIRECTION('center_axis',(-0.974927912181824,0.,-0.222520933956314));
#20387=DIRECTION('ref_axis',(-0.222520933956315,0.,0.974927912181824));
#20388=DIRECTION('center_axis',(-2.7250954951288E-17,-1.,1.19394234705288E-16));
#20389=DIRECTION('ref_axis',(0.222520933956315,-1.22464679914735E-16,-0.974927912181824));
#20390=DIRECTION('center_axis',(-0.78183148246803,0.,0.623489801858734));
#20391=DIRECTION('ref_axis',(0.623489801858733,0.,0.78183148246803));
#20392=DIRECTION('center_axis',(7.63554790147315E-17,-1.,9.57467422477103E-17));
#20393=DIRECTION('ref_axis',(-0.623489801858733,-1.22464679914735E-16,-0.78183148246803));
#20394=DIRECTION('axis',(0.,0.,1.));
#20395=DIRECTION('refdir',(1.,0.,0.));
#20396=DIRECTION('center_axis',(0.974927912181824,0.,-0.222520933956315));
#20397=DIRECTION('ref_axis',(-0.222520933956314,0.,-0.974927912181824));
#20398=DIRECTION('center_axis',(0.,-1.,0.));
#20399=DIRECTION('ref_axis',(0.,0.,-1.));
#20400=DIRECTION('center_axis',(0.,1.,0.));
#20401=DIRECTION('ref_axis',(0.,0.,1.));
#20402=DIRECTION('center_axis',(0.,-1.,0.));
#20403=DIRECTION('ref_axis',(0.,0.,-1.));
#20404=DIRECTION('center_axis',(0.,-1.,0.));
#20405=DIRECTION('ref_axis',(1.,0.,0.));
#20406=DIRECTION('center_axis',(0.,1.,0.));
#20407=DIRECTION('ref_axis',(0.,0.,1.));
#20408=DIRECTION('center_axis',(0.,-1.,0.));
#20409=DIRECTION('ref_axis',(1.,0.,0.));
#20410=DIRECTION('center_axis',(0.,-1.,0.));
#20411=DIRECTION('ref_axis',(1.,0.,0.));
#20412=DIRECTION('center_axis',(0.,-1.,0.));
#20413=DIRECTION('ref_axis',(1.,0.,0.));
#20414=DIRECTION('center_axis',(0.,1.,0.));
#20415=DIRECTION('ref_axis',(0.,0.,1.));
#20416=DIRECTION('center_axis',(0.,-1.,0.));
#20417=DIRECTION('ref_axis',(1.,0.,0.));
#20418=DIRECTION('center_axis',(0.,-1.,0.));
#20419=DIRECTION('ref_axis',(0.,0.,-1.));
#20420=DIRECTION('center_axis',(0.,-1.,0.));
#20421=DIRECTION('ref_axis',(1.,0.,0.));
#20422=DIRECTION('center_axis',(0.78183148246803,0.,0.623489801858734));
#20423=DIRECTION('ref_axis',(0.623489801858734,0.,-0.78183148246803));
#20424=DIRECTION('center_axis',(-0.433883739117558,0.,-0.900968867902419));
#20425=DIRECTION('ref_axis',(-0.900968867902419,0.,0.433883739117558));
#20426=DIRECTION('center_axis',(0.,1.,0.));
#20427=DIRECTION('ref_axis',(0.,0.,1.));
#20428=DIRECTION('center_axis',(0.,-1.,0.));
#20429=DIRECTION('ref_axis',(0.,0.,-1.));
#20430=DIRECTION('center_axis',(0.,1.,0.));
#20431=DIRECTION('ref_axis',(0.,0.,1.));
#20432=DIRECTION('center_axis',(0.,-1.,0.));
#20433=DIRECTION('ref_axis',(1.,0.,0.));
#20434=DIRECTION('center_axis',(0.,-1.,0.));
#20435=DIRECTION('ref_axis',(0.,0.,-1.));
#20436=DIRECTION('center_axis',(0.,-1.,0.));
#20437=DIRECTION('ref_axis',(1.,0.,0.));
#20438=DIRECTION('center_axis',(0.,-1.,0.));
#20439=DIRECTION('ref_axis',(-1.,0.,1.22464679914735E-16));
#20440=DIRECTION('center_axis',(0.,-1.,0.));
#20441=DIRECTION('ref_axis',(1.,0.,0.));
#20442=DIRECTION('center_axis',(0.,-1.,0.));
#20443=DIRECTION('ref_axis',(-1.,0.,1.22464679914735E-16));
#20444=DIRECTION('center_axis',(0.,-1.,0.));
#20445=DIRECTION('ref_axis',(1.,0.,0.));
#20446=DIRECTION('center_axis',(0.,-1.,0.));
#20447=DIRECTION('ref_axis',(0.,0.,-1.));
#20448=DIRECTION('center_axis',(0.,1.,0.));
#20449=DIRECTION('ref_axis',(0.,0.,1.));
#20450=DIRECTION('center_axis',(0.433883739117558,0.,-0.900968867902419));
#20451=DIRECTION('ref_axis',(-0.900968867902419,0.,-0.433883739117558));
#20452=DIRECTION('center_axis',(-0.974927912181824,0.,-0.222520933956315));
#20453=DIRECTION('ref_axis',(-0.222520933956315,0.,0.974927912181824));
#20454=DIRECTION('center_axis',(0.,-1.,0.));
#20455=DIRECTION('ref_axis',(0.,0.,-1.));
#20456=DIRECTION('center_axis',(0.,1.,0.));
#20457=DIRECTION('ref_axis',(0.,0.,1.));
#20458=DIRECTION('center_axis',(0.,-1.,0.));
#20459=DIRECTION('ref_axis',(1.,0.,0.));
#20460=DIRECTION('center_axis',(0.,-1.,0.));
#20461=DIRECTION('ref_axis',(1.,0.,0.));
#20462=DIRECTION('center_axis',(0.,-1.,0.));
#20463=DIRECTION('ref_axis',(1.,0.,0.));
#20464=DIRECTION('center_axis',(0.,-1.,0.));
#20465=DIRECTION('ref_axis',(0.,0.,-1.));
#20466=DIRECTION('center_axis',(0.,1.,0.));
#20467=DIRECTION('ref_axis',(0.,0.,1.));
#20468=DIRECTION('center_axis',(0.,-1.,0.));
#20469=DIRECTION('ref_axis',(1.,0.,0.));
#20470=DIRECTION('center_axis',(0.,1.,0.));
#20471=DIRECTION('ref_axis',(0.,0.,1.));
#20472=DIRECTION('center_axis',(0.,-1.,0.));
#20473=DIRECTION('ref_axis',(1.,0.,0.));
#20474=DIRECTION('center_axis',(0.,-1.,0.));
#20475=DIRECTION('ref_axis',(0.,0.,-1.));
#20476=DIRECTION('center_axis',(0.,-1.,0.));
#20477=DIRECTION('ref_axis',(1.,0.,0.));
#20478=DIRECTION('center_axis',(-0.433883739117558,0.,-0.900968867902419));
#20479=DIRECTION('ref_axis',(-0.900968867902419,0.,0.433883739117558));
#20480=DIRECTION('center_axis',(-0.78183148246803,0.,0.623489801858733));
#20481=DIRECTION('ref_axis',(0.623489801858733,0.,0.78183148246803));
#20482=DIRECTION('center_axis',(0.,-1.,0.));
#20483=DIRECTION('ref_axis',(0.,0.,-1.));
#20484=DIRECTION('center_axis',(0.,1.,0.));
#20485=DIRECTION('ref_axis',(0.,0.,1.));
#20486=DIRECTION('center_axis',(0.,-1.,0.));
#20487=DIRECTION('ref_axis',(1.,0.,0.));
#20488=DIRECTION('center_axis',(0.,-1.,0.));
#20489=DIRECTION('ref_axis',(1.,0.,0.));
#20490=DIRECTION('center_axis',(0.,-1.,0.));
#20491=DIRECTION('ref_axis',(1.,0.,0.));
#20492=DIRECTION('center_axis',(0.,-1.,0.));
#20493=DIRECTION('ref_axis',(0.,0.,-1.));
#20494=DIRECTION('center_axis',(0.,-1.,0.));
#20495=DIRECTION('ref_axis',(1.,0.,0.));
#20496=DIRECTION('center_axis',(0.,1.,0.));
#20497=DIRECTION('ref_axis',(0.,0.,1.));
#20498=DIRECTION('center_axis',(0.,-1.,0.));
#20499=DIRECTION('ref_axis',(1.,0.,0.));
#20500=DIRECTION('center_axis',(0.,-1.,0.));
#20501=DIRECTION('ref_axis',(1.,0.,0.));
#20502=DIRECTION('center_axis',(0.,1.,0.));
#20503=DIRECTION('ref_axis',(0.,0.,1.));
#20504=DIRECTION('center_axis',(0.,-1.,0.));
#20505=DIRECTION('ref_axis',(0.,0.,-1.));
#20506=DIRECTION('center_axis',(0.,0.,1.));
#20507=DIRECTION('ref_axis',(1.,0.,0.));
#20508=DIRECTION('center_axis',(-0.974927912181824,0.,-0.222520933956315));
#20509=DIRECTION('ref_axis',(-0.222520933956315,0.,0.974927912181824));
#20510=DIRECTION('center_axis',(0.,1.,0.));
#20511=DIRECTION('ref_axis',(0.,0.,1.));
#20512=DIRECTION('center_axis',(0.,-1.,0.));
#20513=DIRECTION('ref_axis',(0.,0.,-1.));
#20514=DIRECTION('center_axis',(0.,-1.,0.));
#20515=DIRECTION('ref_axis',(1.,0.,0.));
#20516=DIRECTION('center_axis',(0.,-1.,0.));
#20517=DIRECTION('ref_axis',(1.,0.,0.));
#20518=DIRECTION('center_axis',(0.,-1.,0.));
#20519=DIRECTION('ref_axis',(1.,0.,0.));
#20520=DIRECTION('center_axis',(0.,1.,0.));
#20521=DIRECTION('ref_axis',(0.,0.,1.));
#20522=DIRECTION('center_axis',(0.,-1.,0.));
#20523=DIRECTION('ref_axis',(0.,0.,-1.));
#20524=DIRECTION('center_axis',(0.,-1.,0.));
#20525=DIRECTION('ref_axis',(1.,0.,0.));
#20526=DIRECTION('center_axis',(0.,-1.,0.));
#20527=DIRECTION('ref_axis',(0.,0.,-1.));
#20528=DIRECTION('center_axis',(0.,1.,0.));
#20529=DIRECTION('ref_axis',(0.,0.,1.));
#20530=DIRECTION('center_axis',(0.,-1.,0.));
#20531=DIRECTION('ref_axis',(1.,0.,0.));
#20532=DIRECTION('center_axis',(0.,-1.,0.));
#20533=DIRECTION('ref_axis',(1.,0.,0.));
#20534=DIRECTION('center_axis',(-0.78183148246803,0.,0.623489801858733));
#20535=DIRECTION('ref_axis',(0.623489801858733,0.,0.78183148246803));
#20536=DIRECTION('center_axis',(0.974927912181824,0.,-0.222520933956315));
#20537=DIRECTION('ref_axis',(-0.222520933956314,0.,-0.974927912181824));
#20538=DIRECTION('center_axis',(0.,1.,0.));
#20539=DIRECTION('ref_axis',(0.,0.,1.));
#20540=DIRECTION('center_axis',(0.,-1.,0.));
#20541=DIRECTION('ref_axis',(0.,0.,-1.));
#20542=DIRECTION('center_axis',(0.,-1.,0.));
#20543=DIRECTION('ref_axis',(1.,0.,0.));
#20544=DIRECTION('center_axis',(0.,-1.,0.));
#20545=DIRECTION('ref_axis',(1.,0.,0.));
#20546=DIRECTION('center_axis',(0.,-1.,0.));
#20547=DIRECTION('ref_axis',(1.,0.,0.));
#20548=DIRECTION('center_axis',(0.,1.,0.));
#20549=DIRECTION('ref_axis',(0.,0.,1.));
#20550=DIRECTION('center_axis',(0.,-1.,0.));
#20551=DIRECTION('ref_axis',(0.,0.,-1.));
#20552=DIRECTION('center_axis',(0.,-1.,0.));
#20553=DIRECTION('ref_axis',(1.,0.,0.));
#20554=DIRECTION('center_axis',(0.,-1.,0.));
#20555=DIRECTION('ref_axis',(1.,0.,0.));
#20556=DIRECTION('center_axis',(0.,-1.,0.));
#20557=DIRECTION('ref_axis',(1.,0.,0.));
#20558=DIRECTION('center_axis',(0.,-1.,0.));
#20559=DIRECTION('ref_axis',(0.,0.,-1.));
#20560=DIRECTION('center_axis',(0.,1.,0.));
#20561=DIRECTION('ref_axis',(0.,0.,1.));
#20562=DIRECTION('center_axis',(0.433883739117558,0.,-0.900968867902419));
#20563=DIRECTION('ref_axis',(-0.900968867902419,0.,-0.433883739117558));
#20564=DIRECTION('center_axis',(0.,-1.,0.));
#20565=DIRECTION('ref_axis',(1.,0.,0.));
#20566=DIRECTION('center_axis',(0.,-1.,0.));
#20567=DIRECTION('ref_axis',(1.,0.,0.));
#20568=DIRECTION('center_axis',(0.,-1.,0.));
#20569=DIRECTION('ref_axis',(1.,0.,0.));
#20570=DIRECTION('center_axis',(0.,-1.,0.));
#20571=DIRECTION('ref_axis',(0.,0.,-1.));
#20572=DIRECTION('center_axis',(0.,1.,0.));
#20573=DIRECTION('ref_axis',(0.,0.,1.));
#20574=DIRECTION('center_axis',(0.,1.,0.));
#20575=DIRECTION('ref_axis',(0.,0.,1.));
#20576=DIRECTION('center_axis',(0.,-1.,0.));
#20577=DIRECTION('ref_axis',(1.,0.,0.));
#20578=DIRECTION('center_axis',(0.,0.,1.));
#20579=DIRECTION('ref_axis',(1.,0.,0.));
#20580=DIRECTION('center_axis',(0.,-1.,0.));
#20581=DIRECTION('ref_axis',(0.,0.,-1.));
#20582=DIRECTION('center_axis',(0.,1.,0.));
#20583=DIRECTION('ref_axis',(0.,0.,1.));
#20584=DIRECTION('center_axis',(0.,-1.,0.));
#20585=DIRECTION('ref_axis',(0.,0.,-1.));
#20586=DIRECTION('center_axis',(0.,-1.,0.));
#20587=DIRECTION('ref_axis',(1.,0.,0.));
#20588=DIRECTION('center_axis',(0.,-1.,0.));
#20589=DIRECTION('ref_axis',(1.,0.,0.));
#20590=DIRECTION('center_axis',(0.78183148246803,0.,0.623489801858734));
#20591=DIRECTION('ref_axis',(0.623489801858734,0.,-0.78183148246803));
#20592=DIRECTION('axis',(0.,0.,1.));
#20593=DIRECTION('refdir',(1.,0.,0.));
#20594=DIRECTION('center_axis',(0.,1.,0.));
#20595=DIRECTION('ref_axis',(0.,0.,1.));
#20596=DIRECTION('center_axis',(0.,-1.,0.));
#20597=DIRECTION('ref_axis',(1.,0.,0.));
#20598=DIRECTION('center_axis',(0.,-1.,0.));
#20599=DIRECTION('ref_axis',(1.,0.,0.));
#20600=DIRECTION('center_axis',(0.,-1.,0.));
#20601=DIRECTION('ref_axis',(1.,0.,0.));
#20602=DIRECTION('center_axis',(0.,-1.,0.));
#20603=DIRECTION('ref_axis',(1.,0.,0.));
#20604=DIRECTION('',(0.,1.,0.));
#20605=DIRECTION('center_axis',(0.,-1.,0.));
#20606=DIRECTION('ref_axis',(0.,0.,-1.));
#20607=DIRECTION('center_axis',(0.,-1.,0.));
#20608=DIRECTION('ref_axis',(1.,0.,0.));
#20609=DIRECTION('center_axis',(0.,-1.,0.));
#20610=DIRECTION('ref_axis',(1.,0.,0.));
#20611=DIRECTION('',(0.,1.,0.));
#20612=DIRECTION('center_axis',(0.,1.,0.));
#20613=DIRECTION('ref_axis',(0.,0.,1.));
#20614=DIRECTION('center_axis',(0.,-1.,0.));
#20615=DIRECTION('ref_axis',(1.,0.,0.));
#20616=DIRECTION('center_axis',(0.,-1.,0.));
#20617=DIRECTION('ref_axis',(1.,0.,0.));
#20618=DIRECTION('center_axis',(0.,-1.,0.));
#20619=DIRECTION('ref_axis',(1.,0.,0.));
#20620=DIRECTION('center_axis',(0.,-1.,0.));
#20621=DIRECTION('ref_axis',(1.,0.,0.));
#20622=DIRECTION('',(0.,1.,0.));
#20623=DIRECTION('center_axis',(0.,-1.,0.));
#20624=DIRECTION('ref_axis',(0.,0.,-1.));
#20625=DIRECTION('center_axis',(0.,-1.,0.));
#20626=DIRECTION('ref_axis',(1.,0.,0.));
#20627=DIRECTION('center_axis',(0.,-1.,0.));
#20628=DIRECTION('ref_axis',(1.,0.,0.));
#20629=DIRECTION('',(0.,1.,0.));
#20630=DIRECTION('',(0.,0.,1.));
#20631=DIRECTION('',(1.,0.,0.));
#20632=DIRECTION('',(0.,0.,1.));
#20633=DIRECTION('',(1.,0.,0.));
#20634=DIRECTION('',(0.,0.,1.));
#20635=DIRECTION('',(1.,0.,0.));
#20636=DIRECTION('',(0.,0.,1.));
#20637=DIRECTION('',(1.,0.,0.));
#20638=DIRECTION('',(0.,0.,1.));
#20639=DIRECTION('',(1.,0.,0.));
#20640=DIRECTION('',(0.,0.,1.));
#20641=DIRECTION('',(1.,0.,0.));
#20642=DIRECTION('',(0.,0.,1.));
#20643=DIRECTION('',(1.,0.,0.));
#20644=DIRECTION('',(0.,0.,1.));
#20645=DIRECTION('',(1.,0.,0.));
#20646=DIRECTION('',(0.,0.,1.));
#20647=DIRECTION('',(1.,0.,0.));
#20648=DIRECTION('',(0.,0.,1.));
#20649=DIRECTION('',(1.,0.,0.));
#20650=DIRECTION('',(0.,0.,1.));
#20651=DIRECTION('',(1.,0.,0.));
#20652=DIRECTION('',(0.,0.,1.));
#20653=DIRECTION('',(1.,0.,0.));
#20654=DIRECTION('',(0.,0.,1.));
#20655=DIRECTION('',(1.,0.,0.));
#20656=DIRECTION('',(0.,0.,1.));
#20657=DIRECTION('',(1.,0.,0.));
#20658=DIRECTION('',(0.,0.,1.));
#20659=DIRECTION('',(1.,0.,0.));
#20660=DIRECTION('',(0.,0.,1.));
#20661=DIRECTION('',(1.,0.,0.));
#20662=DIRECTION('',(0.,0.,1.));
#20663=DIRECTION('',(1.,0.,0.));
#20664=DIRECTION('',(0.,0.,1.));
#20665=DIRECTION('',(1.,0.,0.));
#20666=DIRECTION('',(0.,0.,1.));
#20667=DIRECTION('',(1.,0.,0.));
#20668=DIRECTION('',(0.,0.,1.));
#20669=DIRECTION('',(1.,0.,0.));
#20670=DIRECTION('',(0.,0.,1.));
#20671=DIRECTION('',(1.,0.,0.));
#20672=DIRECTION('',(0.,0.,1.));
#20673=DIRECTION('',(1.,0.,0.));
#20674=DIRECTION('',(0.,-1.,2.22044604925031E-16));
#20675=DIRECTION('',(1.,0.,0.));
#20676=DIRECTION('',(0.,-1.,2.22044604925031E-16));
#20677=DIRECTION('',(1.,0.,0.));
#20678=DIRECTION('',(0.,-1.,2.22044604925031E-16));
#20679=DIRECTION('',(1.,0.,0.));
#20680=DIRECTION('',(0.,-1.,2.22044604925031E-16));
#20681=DIRECTION('',(1.,0.,0.));
#20682=DIRECTION('',(0.,0.,1.));
#20683=DIRECTION('',(2.22044604925031E-16,-1.,0.));
#20684=DIRECTION('',(0.,0.,1.));
#20685=DIRECTION('',(2.22044604925031E-16,1.,0.));
#20686=DIRECTION('',(0.,0.,1.));
#20687=DIRECTION('',(2.22044604925031E-16,1.,0.));
#20688=DIRECTION('',(0.,0.,1.));
#20689=DIRECTION('',(2.22044604925031E-16,1.,0.));
#20690=DIRECTION('',(0.,0.,1.));
#20691=DIRECTION('',(2.22044604925031E-16,1.,0.));
#20692=DIRECTION('',(0.,0.,1.));
#20693=DIRECTION('',(2.22044604925031E-16,-1.,0.));
#20694=DIRECTION('',(0.,0.,1.));
#20695=DIRECTION('',(2.22044604925031E-16,-1.,0.));
#20696=DIRECTION('',(0.,0.,1.));
#20697=DIRECTION('',(2.22044604925031E-16,-1.,0.));
#20698=DIRECTION('',(0.,0.,1.));
#20699=DIRECTION('',(2.22044604925031E-16,-1.,0.));
#20700=DIRECTION('',(0.,-1.,2.22044604925031E-16));
#20701=DIRECTION('',(1.,0.,0.));
#20702=DIRECTION('',(0.,-1.,2.22044604925031E-16));
#20703=DIRECTION('',(1.,0.,0.));
#20704=DIRECTION('',(0.,-1.,2.22044604925031E-16));
#20705=DIRECTION('',(1.,0.,0.));
#20706=DIRECTION('',(0.,-1.,2.22044604925031E-16));
#20707=DIRECTION('',(1.,0.,0.));
#20708=DIRECTION('',(0.,0.,1.));
#20709=DIRECTION('',(2.22044604925031E-16,-1.,0.));
#20710=DIRECTION('',(0.,0.,1.));
#20711=DIRECTION('',(2.22044604925031E-16,1.,0.));
#20712=DIRECTION('',(0.,0.,1.));
#20713=DIRECTION('',(2.22044604925031E-16,1.,0.));
#20714=DIRECTION('',(0.,0.,1.));
#20715=DIRECTION('',(2.22044604925031E-16,1.,0.));
#20716=DIRECTION('',(0.,0.,1.));
#20717=DIRECTION('',(2.22044604925031E-16,1.,0.));
#20718=DIRECTION('',(0.,0.,1.));
#20719=DIRECTION('',(2.22044604925031E-16,-1.,0.));
#20720=DIRECTION('',(0.,0.,1.));
#20721=DIRECTION('',(2.22044604925031E-16,-1.,0.));
#20722=DIRECTION('',(0.,0.,1.));
#20723=DIRECTION('',(2.22044604925031E-16,-1.,0.));
#20724=DIRECTION('',(0.,0.,1.));
#20725=DIRECTION('',(2.22044604925031E-16,-1.,0.));
#20726=DIRECTION('',(0.,0.,1.));
#20727=DIRECTION('',(-1.,1.22464679914735E-16,0.));
#20728=DIRECTION('',(0.,0.,1.));
#20729=DIRECTION('',(1.,0.,0.));
#20730=DIRECTION('',(0.,0.,1.));
#20731=DIRECTION('',(1.,0.,0.));
#20732=DIRECTION('',(0.,0.,1.));
#20733=DIRECTION('',(1.,0.,0.));
#20734=DIRECTION('',(0.,0.,1.));
#20735=DIRECTION('',(1.,0.,0.));
#20736=DIRECTION('',(0.,0.,1.));
#20737=DIRECTION('',(1.,0.,0.));
#20738=DIRECTION('',(0.,0.,1.));
#20739=DIRECTION('',(1.,0.,0.));
#20740=DIRECTION('',(0.,0.,1.));
#20741=DIRECTION('',(1.,0.,0.));
#20742=DIRECTION('',(0.,0.,1.));
#20743=DIRECTION('',(1.,0.,0.));
#20744=DIRECTION('',(0.,0.,1.));
#20745=DIRECTION('',(1.,0.,0.));
#20746=DIRECTION('',(0.,0.,1.));
#20747=DIRECTION('',(1.,0.,0.));
#20748=DIRECTION('',(0.,0.,1.));
#20749=DIRECTION('',(1.,0.,0.));
#20750=DIRECTION('',(0.,0.,1.));
#20751=DIRECTION('',(1.,0.,0.));
#20752=DIRECTION('',(0.,0.,1.));
#20753=DIRECTION('',(1.,0.,0.));
#20754=DIRECTION('',(0.,0.,1.));
#20755=DIRECTION('',(1.,0.,0.));
#20756=DIRECTION('',(0.,0.,1.));
#20757=DIRECTION('',(1.,0.,0.));
#20758=DIRECTION('',(0.,0.,1.));
#20759=DIRECTION('',(1.,0.,0.));
#20760=DIRECTION('',(0.,0.,1.));
#20761=DIRECTION('',(1.,0.,0.));
#20762=DIRECTION('',(0.,0.,1.));
#20763=DIRECTION('',(1.,0.,0.));
#20764=DIRECTION('',(0.,0.,1.));
#20765=DIRECTION('',(1.,0.,0.));
#20766=DIRECTION('',(0.,0.,1.));
#20767=DIRECTION('',(1.,0.,0.));
#20768=DIRECTION('',(0.,0.,1.));
#20769=DIRECTION('',(1.,0.,0.));
#20770=DIRECTION('',(0.,0.,1.));
#20771=DIRECTION('',(1.,0.,0.));
#20772=DIRECTION('',(0.,0.,1.));
#20773=DIRECTION('',(1.,0.,0.));
#20774=DIRECTION('',(0.,0.,1.));
#20775=DIRECTION('',(1.,0.,0.));
#20776=DIRECTION('',(0.,0.,1.));
#20777=DIRECTION('',(1.,0.,0.));
#20778=DIRECTION('',(0.,0.,1.));
#20779=DIRECTION('',(1.,0.,0.));
#20780=DIRECTION('',(0.,0.,1.));
#20781=DIRECTION('',(1.,0.,0.));
#20782=DIRECTION('',(0.,0.,1.));
#20783=DIRECTION('',(1.,0.,0.));
#20784=DIRECTION('',(0.,0.,1.));
#20785=DIRECTION('',(1.,0.,0.));
#20786=DIRECTION('axis',(0.,0.,1.));
#20787=DIRECTION('refdir',(1.,0.,0.));
#20788=DIRECTION('axis',(0.,0.,1.));
#20789=DIRECTION('refdir',(1.,0.,0.));
#20790=DIRECTION('center_axis',(1.,0.,0.));
#20791=DIRECTION('ref_axis',(0.,0.,-1.));
#20792=DIRECTION('center_axis',(1.,0.,0.));
#20793=DIRECTION('ref_axis',(0.,0.,-1.));
#20794=DIRECTION('center_axis',(1.,0.,0.));
#20795=DIRECTION('ref_axis',(0.,0.,-1.));
#20796=DIRECTION('center_axis',(1.,0.,0.));
#20797=DIRECTION('ref_axis',(0.,0.,-1.));
#20798=DIRECTION('center_axis',(1.,0.,0.));
#20799=DIRECTION('ref_axis',(0.,0.,-1.));
#20800=DIRECTION('center_axis',(-1.,0.,0.));
#20801=DIRECTION('ref_axis',(0.,0.,-1.));
#20802=DIRECTION('center_axis',(1.,0.,0.));
#20803=DIRECTION('ref_axis',(0.,0.,-1.));
#20804=DIRECTION('',(-1.,0.,0.));
#20805=DIRECTION('center_axis',(1.,0.,0.));
#20806=DIRECTION('ref_axis',(0.,0.,-1.));
#20807=DIRECTION('',(-1.,0.,0.));
#20808=DIRECTION('center_axis',(1.,0.,0.));
#20809=DIRECTION('ref_axis',(0.,0.,-1.));
#20810=DIRECTION('center_axis',(1.,0.,0.));
#20811=DIRECTION('ref_axis',(0.,0.,-1.));
#20812=DIRECTION('center_axis',(1.,0.,0.));
#20813=DIRECTION('ref_axis',(0.,0.,-1.));
#20814=DIRECTION('center_axis',(1.,0.,0.));
#20815=DIRECTION('ref_axis',(0.,0.,-1.));
#20816=DIRECTION('center_axis',(1.,0.,0.));
#20817=DIRECTION('ref_axis',(0.,0.,-1.));
#20818=DIRECTION('center_axis',(-1.,0.,0.));
#20819=DIRECTION('ref_axis',(0.,0.,-1.));
#20820=DIRECTION('center_axis',(1.,0.,0.));
#20821=DIRECTION('ref_axis',(0.,0.,-1.));
#20822=DIRECTION('',(-1.,0.,0.));
#20823=DIRECTION('center_axis',(1.,0.,0.));
#20824=DIRECTION('ref_axis',(0.,0.,-1.));
#20825=DIRECTION('',(-1.,0.,0.));
#20826=DIRECTION('center_axis',(1.,0.,0.));
#20827=DIRECTION('ref_axis',(0.,0.,-1.));
#20828=DIRECTION('center_axis',(1.,0.,0.));
#20829=DIRECTION('ref_axis',(0.,0.,-1.));
#20830=DIRECTION('center_axis',(1.,0.,0.));
#20831=DIRECTION('ref_axis',(0.,0.,-1.));
#20832=DIRECTION('',(-1.,0.,0.));
#20833=DIRECTION('center_axis',(1.,0.,0.));
#20834=DIRECTION('ref_axis',(0.,0.,-1.));
#20835=DIRECTION('center_axis',(1.,0.,0.));
#20836=DIRECTION('ref_axis',(0.,0.,-1.));
#20837=DIRECTION('axis',(0.,0.,1.));
#20838=DIRECTION('refdir',(1.,0.,0.));
#20839=DIRECTION('center_axis',(1.,0.,0.));
#20840=DIRECTION('ref_axis',(0.,0.,-1.));
#20841=DIRECTION('center_axis',(-1.,0.,0.));
#20842=DIRECTION('ref_axis',(0.,0.,-1.));
#20843=DIRECTION('',(-1.,0.,0.));
#20844=DIRECTION('center_axis',(-1.,0.,0.));
#20845=DIRECTION('ref_axis',(0.,0.,-1.));
#20846=DIRECTION('center_axis',(1.,0.,0.));
#20847=DIRECTION('ref_axis',(0.,0.,-1.));
#20848=DIRECTION('center_axis',(1.,0.,0.));
#20849=DIRECTION('ref_axis',(0.,0.,-1.));
#20850=DIRECTION('',(-1.,0.,0.));
#20851=DIRECTION('center_axis',(1.,0.,0.));
#20852=DIRECTION('ref_axis',(0.,0.,-1.));
#20853=DIRECTION('center_axis',(1.,0.,0.));
#20854=DIRECTION('ref_axis',(0.,0.,-1.));
#20855=DIRECTION('center_axis',(1.,0.,0.));
#20856=DIRECTION('ref_axis',(0.,0.,-1.));
#20857=DIRECTION('axis',(0.,0.,1.));
#20858=DIRECTION('refdir',(1.,0.,0.));
#20859=DIRECTION('center_axis',(1.,0.,0.));
#20860=DIRECTION('ref_axis',(0.,0.,-1.));
#20861=DIRECTION('center_axis',(-1.,0.,0.));
#20862=DIRECTION('ref_axis',(0.,0.,-1.));
#20863=DIRECTION('',(-1.,0.,0.));
#20864=DIRECTION('center_axis',(-1.,0.,0.));
#20865=DIRECTION('ref_axis',(0.,0.,-1.));
#20866=DIRECTION('center_axis',(1.,0.,0.));
#20867=DIRECTION('ref_axis',(0.,0.,-1.));
#20868=DIRECTION('center_axis',(1.,0.,0.));
#20869=DIRECTION('ref_axis',(0.,0.,-1.));
#20870=DIRECTION('',(-1.,0.,0.));
#20871=DIRECTION('center_axis',(1.,0.,0.));
#20872=DIRECTION('ref_axis',(0.,0.,-1.));
#20873=DIRECTION('center_axis',(1.,0.,0.));
#20874=DIRECTION('ref_axis',(0.,0.,-1.));
#20875=DIRECTION('center_axis',(1.,0.,0.));
#20876=DIRECTION('ref_axis',(0.,0.,-1.));
#20877=DIRECTION('axis',(0.,0.,1.));
#20878=DIRECTION('refdir',(1.,0.,0.));
#20879=DIRECTION('center_axis',(1.,0.,0.));
#20880=DIRECTION('ref_axis',(0.,0.,-1.));
#20881=DIRECTION('center_axis',(-1.,0.,0.));
#20882=DIRECTION('ref_axis',(0.,0.,-1.));
#20883=DIRECTION('',(-1.,0.,0.));
#20884=DIRECTION('center_axis',(-1.,0.,0.));
#20885=DIRECTION('ref_axis',(0.,0.,-1.));
#20886=DIRECTION('center_axis',(1.,0.,0.));
#20887=DIRECTION('ref_axis',(0.,0.,-1.));
#20888=DIRECTION('center_axis',(1.,0.,0.));
#20889=DIRECTION('ref_axis',(0.,0.,-1.));
#20890=DIRECTION('',(-1.,0.,0.));
#20891=DIRECTION('center_axis',(1.,0.,0.));
#20892=DIRECTION('ref_axis',(0.,0.,-1.));
#20893=DIRECTION('center_axis',(1.,0.,0.));
#20894=DIRECTION('ref_axis',(0.,0.,-1.));
#20895=DIRECTION('center_axis',(1.,0.,0.));
#20896=DIRECTION('ref_axis',(0.,0.,-1.));
#20897=DIRECTION('axis',(0.,0.,1.));
#20898=DIRECTION('refdir',(1.,0.,0.));
#20899=DIRECTION('center_axis',(1.,0.,0.));
#20900=DIRECTION('ref_axis',(0.,0.,-1.));
#20901=DIRECTION('center_axis',(-1.,0.,0.));
#20902=DIRECTION('ref_axis',(0.,0.,-1.));
#20903=DIRECTION('',(-1.,0.,0.));
#20904=DIRECTION('center_axis',(-1.,0.,0.));
#20905=DIRECTION('ref_axis',(0.,0.,-1.));
#20906=DIRECTION('center_axis',(1.,0.,0.));
#20907=DIRECTION('ref_axis',(0.,0.,-1.));
#20908=DIRECTION('center_axis',(1.,0.,0.));
#20909=DIRECTION('ref_axis',(0.,0.,-1.));
#20910=DIRECTION('',(-1.,0.,0.));
#20911=DIRECTION('center_axis',(1.,0.,0.));
#20912=DIRECTION('ref_axis',(0.,0.,-1.));
#20913=DIRECTION('center_axis',(1.,0.,0.));
#20914=DIRECTION('ref_axis',(0.,0.,-1.));
#20915=DIRECTION('center_axis',(1.,0.,0.));
#20916=DIRECTION('ref_axis',(0.,0.,-1.));
#20917=DIRECTION('axis',(0.,0.,1.));
#20918=DIRECTION('refdir',(1.,0.,0.));
#20919=DIRECTION('center_axis',(1.,0.,0.));
#20920=DIRECTION('ref_axis',(0.,0.,-1.));
#20921=DIRECTION('center_axis',(1.,0.,0.));
#20922=DIRECTION('ref_axis',(0.,0.,-1.));
#20923=DIRECTION('',(-1.,0.,0.));
#20924=DIRECTION('center_axis',(1.,0.,0.));
#20925=DIRECTION('ref_axis',(0.,0.,-1.));
#20926=DIRECTION('center_axis',(1.,0.,0.));
#20927=DIRECTION('ref_axis',(0.,0.,-1.));
#20928=DIRECTION('center_axis',(1.,0.,0.));
#20929=DIRECTION('ref_axis',(0.,0.,-1.));
#20930=DIRECTION('center_axis',(-1.,0.,0.));
#20931=DIRECTION('ref_axis',(0.,0.,-1.));
#20932=DIRECTION('',(-1.,0.,0.));
#20933=DIRECTION('center_axis',(-1.,0.,0.));
#20934=DIRECTION('ref_axis',(0.,0.,-1.));
#20935=DIRECTION('center_axis',(1.,0.,0.));
#20936=DIRECTION('ref_axis',(0.,0.,-1.));
#20937=DIRECTION('center_axis',(1.,0.,0.));
#20938=DIRECTION('ref_axis',(0.,0.,-1.));
#20939=DIRECTION('',(-1.,0.,0.));
#20940=DIRECTION('center_axis',(1.,0.,0.));
#20941=DIRECTION('ref_axis',(0.,0.,-1.));
#20942=DIRECTION('center_axis',(1.,0.,0.));
#20943=DIRECTION('ref_axis',(0.,0.,-1.));
#20944=DIRECTION('center_axis',(1.,0.,0.));
#20945=DIRECTION('ref_axis',(0.,0.,-1.));
#20946=DIRECTION('',(0.,0.,1.));
#20947=DIRECTION('',(1.,0.,0.));
#20948=DIRECTION('',(0.,0.,1.));
#20949=DIRECTION('',(1.,0.,0.));
#20950=DIRECTION('',(0.,0.,1.));
#20951=DIRECTION('',(1.,0.,0.));
#20952=DIRECTION('',(0.,0.,1.));
#20953=DIRECTION('',(1.,0.,0.));
#20954=DIRECTION('',(0.,0.,1.));
#20955=DIRECTION('',(1.,0.,0.));
#20956=DIRECTION('',(0.,0.,1.));
#20957=DIRECTION('',(1.,0.,0.));
#20958=DIRECTION('',(0.,0.,1.));
#20959=DIRECTION('',(1.,0.,0.));
#20960=DIRECTION('',(6.12323399573677E-17,0.,1.));
#20961=DIRECTION('',(1.,1.20569138793732E-97,-6.12323399573677E-17));
#20962=DIRECTION('',(6.12323399573677E-17,0.,1.));
#20963=DIRECTION('',(1.,5.27090436347397E-98,-6.12323399573677E-17));
#20964=DIRECTION('',(6.12323399573677E-17,0.,1.));
#20965=DIRECTION('',(1.,6.78600951589921E-98,-6.12323399573677E-17));
#20966=DIRECTION('',(-0.148647713313796,-4.34599535207206E-18,0.988890215001993));
#20967=DIRECTION('',(0.988890215001957,2.92853616645372E-17,0.148647713313791));
#20968=DIRECTION('',(0.148647713313796,-6.67175965354258E-18,0.988890215001993));
#20969=DIRECTION('',(0.988890215001957,-4.49574559025405E-17,-0.148647713313791));
#20970=DIRECTION('',(-8.62516084659135E-17,0.641333040047924,-0.767262622407015));
#20971=DIRECTION('',(0.999999999999999,6.12323399573676E-17,-6.12323399573676E-17));
#20972=DIRECTION('center_axis',(0.,0.,1.));
#20973=DIRECTION('ref_axis',(1.,0.,0.));
#20974=CARTESIAN_POINT('',(0.,0.,0.));
#20975=CARTESIAN_POINT('',(0.,0.,0.));
#20976=CARTESIAN_POINT('',(0.,0.,0.));
#20977=CARTESIAN_POINT('Origin',(46.5,-4.,-0.1));
#20978=CARTESIAN_POINT('',(46.29,-4.,0.));
#20979=CARTESIAN_POINT('Origin',(46.5,-4.,0.));
#20980=CARTESIAN_POINT('',(46.29,-4.,1.));
#20981=CARTESIAN_POINT('',(46.29,-4.,-0.1));
#20982=CARTESIAN_POINT('Origin',(46.5,-4.,1.));
#20983=CARTESIAN_POINT('Origin',(43.5,4.,-0.1));
#20984=CARTESIAN_POINT('',(43.29,4.,0.));
#20985=CARTESIAN_POINT('Origin',(43.5,4.,0.));
#20986=CARTESIAN_POINT('',(43.29,4.,1.));
#20987=CARTESIAN_POINT('',(43.29,4.,-0.1));
#20988=CARTESIAN_POINT('Origin',(43.5,4.,1.));
#20989=CARTESIAN_POINT('Origin',(43.5,-4.,-0.1));
#20990=CARTESIAN_POINT('',(43.29,-4.,0.));
#20991=CARTESIAN_POINT('Origin',(43.5,-4.,0.));
#20992=CARTESIAN_POINT('',(43.29,-4.,1.));
#20993=CARTESIAN_POINT('',(43.29,-4.,-0.1));
#20994=CARTESIAN_POINT('Origin',(43.5,-4.,1.));
#20995=CARTESIAN_POINT('Origin',(46.5,4.,-0.1));
#20996=CARTESIAN_POINT('',(46.29,4.,0.));
#20997=CARTESIAN_POINT('Origin',(46.5,4.,0.));
#20998=CARTESIAN_POINT('',(46.29,4.,1.));
#20999=CARTESIAN_POINT('',(46.29,4.,-0.1));
#21000=CARTESIAN_POINT('Origin',(46.5,4.,1.));
#21001=CARTESIAN_POINT('Origin',(1.5,-4.,-0.1));
#21002=CARTESIAN_POINT('',(1.29,-4.,0.));
#21003=CARTESIAN_POINT('Origin',(1.5,-4.,0.));
#21004=CARTESIAN_POINT('',(1.29,-4.,1.));
#21005=CARTESIAN_POINT('',(1.29,-4.,-0.1));
#21006=CARTESIAN_POINT('Origin',(1.5,-4.,1.));
#21007=CARTESIAN_POINT('Origin',(-1.5,4.,-0.1));
#21008=CARTESIAN_POINT('',(-1.71,4.,0.));
#21009=CARTESIAN_POINT('Origin',(-1.5,4.,0.));
#21010=CARTESIAN_POINT('',(-1.71,4.,1.));
#21011=CARTESIAN_POINT('',(-1.71,4.,-0.1));
#21012=CARTESIAN_POINT('Origin',(-1.5,4.,1.));
#21013=CARTESIAN_POINT('Origin',(-1.5,-4.,-0.1));
#21014=CARTESIAN_POINT('',(-1.71,-4.,0.));
#21015=CARTESIAN_POINT('Origin',(-1.5,-4.,0.));
#21016=CARTESIAN_POINT('',(-1.71,-4.,1.));
#21017=CARTESIAN_POINT('',(-1.71,-4.,-0.1));
#21018=CARTESIAN_POINT('Origin',(-1.5,-4.,1.));
#21019=CARTESIAN_POINT('Origin',(1.5,4.,-0.1));
#21020=CARTESIAN_POINT('',(1.29,4.,0.));
#21021=CARTESIAN_POINT('Origin',(1.5,4.,0.));
#21022=CARTESIAN_POINT('',(1.29,4.,1.));
#21023=CARTESIAN_POINT('',(1.29,4.,-0.1));
#21024=CARTESIAN_POINT('Origin',(1.5,4.,1.));
#21025=CARTESIAN_POINT('Origin',(48.,10.,0.));
#21026=CARTESIAN_POINT('',(48.,10.,0.));
#21027=CARTESIAN_POINT('',(-3.,10.,0.));
#21028=CARTESIAN_POINT('',(48.,10.,0.));
#21029=CARTESIAN_POINT('',(-3.,10.,1.));
#21030=CARTESIAN_POINT('',(-3.,10.,0.));
#21031=CARTESIAN_POINT('',(48.,10.,1.));
#21032=CARTESIAN_POINT('',(48.,10.,1.));
#21033=CARTESIAN_POINT('',(48.,10.,0.));
#21034=CARTESIAN_POINT('Origin',(48.,-10.,0.));
#21035=CARTESIAN_POINT('',(48.,-10.,0.));
#21036=CARTESIAN_POINT('',(48.,-10.,0.));
#21037=CARTESIAN_POINT('',(48.,-10.,1.));
#21038=CARTESIAN_POINT('',(48.,-10.,1.));
#21039=CARTESIAN_POINT('',(48.,-10.,0.));
#21040=CARTESIAN_POINT('Origin',(-3.,-10.,0.));
#21041=CARTESIAN_POINT('',(-3.,-10.,0.));
#21042=CARTESIAN_POINT('',(-3.,-10.,0.));
#21043=CARTESIAN_POINT('',(-3.,-10.,1.));
#21044=CARTESIAN_POINT('',(-3.,-10.,1.));
#21045=CARTESIAN_POINT('',(-3.,-10.,0.));
#21046=CARTESIAN_POINT('Origin',(-3.,10.,0.));
#21047=CARTESIAN_POINT('',(-3.,10.,0.));
#21048=CARTESIAN_POINT('',(-3.,10.,1.));
#21049=CARTESIAN_POINT('Origin',(22.5,0.,1.));
#21050=CARTESIAN_POINT('Origin',(22.5,0.,0.));
#21051=CARTESIAN_POINT('',(0.,0.,0.));
#21052=CARTESIAN_POINT('Origin',(-2.,10.,-0.8));
#21053=CARTESIAN_POINT('',(-2.,10.,-1.8));
#21054=CARTESIAN_POINT('',(-3.,10.,-1.8));
#21055=CARTESIAN_POINT('',(-2.25,10.,-1.8));
#21056=CARTESIAN_POINT('',(-3.,10.,0.));
#21057=CARTESIAN_POINT('',(-3.,10.,-0.8));
#21058=CARTESIAN_POINT('',(-2.,10.,0.));
#21059=CARTESIAN_POINT('',(-2.,10.,0.));
#21060=CARTESIAN_POINT('',(-2.,10.,-0.8));
#21061=CARTESIAN_POINT('Origin',(-2.,-10.,-0.8));
#21062=CARTESIAN_POINT('',(-2.,-10.,-1.8));
#21063=CARTESIAN_POINT('',(-2.,-5.,-1.8));
#21064=CARTESIAN_POINT('',(-2.,-10.,0.));
#21065=CARTESIAN_POINT('',(-2.,-10.,0.));
#21066=CARTESIAN_POINT('',(-2.,-10.,-0.8));
#21067=CARTESIAN_POINT('Origin',(-3.,-10.,-0.8));
#21068=CARTESIAN_POINT('',(-3.,-10.,-1.8));
#21069=CARTESIAN_POINT('',(-2.75,-10.,-1.8));
#21070=CARTESIAN_POINT('',(-3.,-10.,0.));
#21071=CARTESIAN_POINT('',(-3.,-10.,0.));
#21072=CARTESIAN_POINT('',(-3.,-10.,-0.8));
#21073=CARTESIAN_POINT('Origin',(-3.,10.,-0.8));
#21074=CARTESIAN_POINT('',(-3.,5.,-1.8));
#21075=CARTESIAN_POINT('',(-3.,10.,0.));
#21076=CARTESIAN_POINT('Origin',(-2.5,0.,0.));
#21077=CARTESIAN_POINT('Origin',(-2.5,0.,-1.8));
#21078=CARTESIAN_POINT('',(0.,0.,0.));
#21079=CARTESIAN_POINT('Origin',(48.,10.,-0.8));
#21080=CARTESIAN_POINT('',(48.,10.,-1.8));
#21081=CARTESIAN_POINT('',(47.,10.,-1.8));
#21082=CARTESIAN_POINT('',(47.75,10.,-1.8));
#21083=CARTESIAN_POINT('',(47.,10.,0.));
#21084=CARTESIAN_POINT('',(47.,10.,-0.8));
#21085=CARTESIAN_POINT('',(48.,10.,0.));
#21086=CARTESIAN_POINT('',(48.,10.,0.));
#21087=CARTESIAN_POINT('',(48.,10.,-0.8));
#21088=CARTESIAN_POINT('Origin',(48.,-10.,-0.8));
#21089=CARTESIAN_POINT('',(48.,-10.,-1.8));
#21090=CARTESIAN_POINT('',(48.,-5.,-1.8));
#21091=CARTESIAN_POINT('',(48.,-10.,0.));
#21092=CARTESIAN_POINT('',(48.,-10.,0.));
#21093=CARTESIAN_POINT('',(48.,-10.,-0.8));
#21094=CARTESIAN_POINT('Origin',(47.,-10.,-0.8));
#21095=CARTESIAN_POINT('',(47.,-10.,-1.8));
#21096=CARTESIAN_POINT('',(47.25,-10.,-1.8));
#21097=CARTESIAN_POINT('',(47.,-10.,0.));
#21098=CARTESIAN_POINT('',(47.,-10.,0.));
#21099=CARTESIAN_POINT('',(47.,-10.,-0.8));
#21100=CARTESIAN_POINT('Origin',(47.,10.,-0.8));
#21101=CARTESIAN_POINT('',(47.,5.,-1.8));
#21102=CARTESIAN_POINT('',(47.,10.,0.));
#21103=CARTESIAN_POINT('Origin',(47.5,0.,0.));
#21104=CARTESIAN_POINT('Origin',(47.5,0.,-1.8));
#21105=CARTESIAN_POINT('',(0.,0.,0.));
#21106=CARTESIAN_POINT('Origin',(-1.1,-1.30814754519511,4.69185245480489));
#21107=CARTESIAN_POINT('',(-1.,-1.30814754519511,4.85685245480489));
#21108=CARTESIAN_POINT('Origin',(-1.,-1.30814754519511,4.69185245480489));
#21109=CARTESIAN_POINT('',(1.,-1.30814754519511,4.85685245480489));
#21110=CARTESIAN_POINT('',(-1.1,-1.30814754519511,4.85685245480489));
#21111=CARTESIAN_POINT('Origin',(1.,-1.30814754519511,4.69185245480489));
#21112=CARTESIAN_POINT('Origin',(-1.1,-1.30814754519511,7.30814754519511));
#21113=CARTESIAN_POINT('',(-1.,-1.30814754519511,7.47314754519511));
#21114=CARTESIAN_POINT('Origin',(-1.,-1.30814754519511,7.30814754519511));
#21115=CARTESIAN_POINT('',(1.,-1.30814754519511,7.47314754519511));
#21116=CARTESIAN_POINT('',(-1.1,-1.30814754519511,7.47314754519511));
#21117=CARTESIAN_POINT('Origin',(1.,-1.30814754519511,7.30814754519511));
#21118=CARTESIAN_POINT('Origin',(-1.1,1.30814754519511,7.30814754519511));
#21119=CARTESIAN_POINT('',(-1.,1.30814754519511,7.47314754519511));
#21120=CARTESIAN_POINT('Origin',(-1.,1.30814754519511,7.30814754519511));
#21121=CARTESIAN_POINT('',(1.,1.30814754519511,7.47314754519511));
#21122=CARTESIAN_POINT('',(-1.1,1.30814754519511,7.47314754519511));
#21123=CARTESIAN_POINT('Origin',(1.,1.30814754519511,7.30814754519511));
#21124=CARTESIAN_POINT('Origin',(-1.1,1.30814754519511,4.69185245480489));
#21125=CARTESIAN_POINT('',(-1.,1.30814754519511,4.85685245480489));
#21126=CARTESIAN_POINT('Origin',(-1.,1.30814754519511,4.69185245480489));
#21127=CARTESIAN_POINT('',(1.,1.30814754519511,4.85685245480489));
#21128=CARTESIAN_POINT('',(-1.1,1.30814754519511,4.85685245480489));
#21129=CARTESIAN_POINT('Origin',(1.,1.30814754519511,4.69185245480489));
#21130=CARTESIAN_POINT('Origin',(-1.1,0.,6.));
#21131=CARTESIAN_POINT('',(-1.,-1.95943487863576E-16,7.6));
#21132=CARTESIAN_POINT('Origin',(-1.,0.,6.));
#21133=CARTESIAN_POINT('',(1.,1.95943487863576E-16,7.6));
#21134=CARTESIAN_POINT('',(-1.1,-1.95943487863576E-16,7.6));
#21135=CARTESIAN_POINT('Origin',(1.,0.,6.));
#21136=CARTESIAN_POINT('Origin',(1.5,-4.,0.9));
#21137=CARTESIAN_POINT('',(1.225,-4.,1.));
#21138=CARTESIAN_POINT('Origin',(1.5,-4.,1.));
#21139=CARTESIAN_POINT('',(1.225,-4.,2.));
#21140=CARTESIAN_POINT('',(1.225,-4.,0.9));
#21141=CARTESIAN_POINT('Origin',(1.5,-4.,2.));
#21142=CARTESIAN_POINT('Origin',(-1.5,4.,0.9));
#21143=CARTESIAN_POINT('',(-1.775,4.,1.));
#21144=CARTESIAN_POINT('Origin',(-1.5,4.,1.));
#21145=CARTESIAN_POINT('',(-1.775,4.,2.));
#21146=CARTESIAN_POINT('',(-1.775,4.,0.9));
#21147=CARTESIAN_POINT('Origin',(-1.5,4.,2.));
#21148=CARTESIAN_POINT('Origin',(-1.5,-4.,0.9));
#21149=CARTESIAN_POINT('',(-1.775,-4.,1.));
#21150=CARTESIAN_POINT('Origin',(-1.5,-4.,1.));
#21151=CARTESIAN_POINT('',(-1.775,-4.,2.));
#21152=CARTESIAN_POINT('',(-1.775,-4.,0.9));
#21153=CARTESIAN_POINT('Origin',(-1.5,-4.,2.));
#21154=CARTESIAN_POINT('Origin',(1.5,4.,0.9));
#21155=CARTESIAN_POINT('',(1.225,4.,1.));
#21156=CARTESIAN_POINT('Origin',(1.5,4.,1.));
#21157=CARTESIAN_POINT('',(1.225,4.,2.));
#21158=CARTESIAN_POINT('',(1.225,4.,0.9));
#21159=CARTESIAN_POINT('Origin',(1.5,4.,2.));
#21160=CARTESIAN_POINT('Origin',(0.,0.,2.));
#21161=CARTESIAN_POINT('',(-1.,5.,2.));
#21162=CARTESIAN_POINT('',(-1.,-5.,2.));
#21163=CARTESIAN_POINT('',(-1.,2.5,2.));
#21164=CARTESIAN_POINT('',(-2.,5.,2.));
#21165=CARTESIAN_POINT('',(2.,5.,2.));
#21166=CARTESIAN_POINT('',(-2.,-5.,2.));
#21167=CARTESIAN_POINT('',(-2.,5.,2.));
#21168=CARTESIAN_POINT('',(-2.,-5.,2.));
#21169=CARTESIAN_POINT('Origin',(0.,0.,2.));
#21170=CARTESIAN_POINT('',(1.,-5.,2.));
#21171=CARTESIAN_POINT('',(1.,5.,2.));
#21172=CARTESIAN_POINT('',(1.,-2.5,2.));
#21173=CARTESIAN_POINT('',(2.,-5.,2.));
#21174=CARTESIAN_POINT('',(-2.,-5.,2.));
#21175=CARTESIAN_POINT('',(2.,5.,2.));
#21176=CARTESIAN_POINT('',(2.,-5.,2.));
#21177=CARTESIAN_POINT('',(2.,5.,2.));
#21178=CARTESIAN_POINT('Origin',(2.,-5.,1.));
#21179=CARTESIAN_POINT('',(2.,-5.,1.));
#21180=CARTESIAN_POINT('',(2.,5.,1.));
#21181=CARTESIAN_POINT('',(2.,-5.,1.));
#21182=CARTESIAN_POINT('',(2.,5.,1.));
#21183=CARTESIAN_POINT('',(2.,-5.,1.));
#21184=CARTESIAN_POINT('Origin',(-2.,5.,1.));
#21185=CARTESIAN_POINT('',(-2.,5.,1.));
#21186=CARTESIAN_POINT('',(-2.,-5.,1.));
#21187=CARTESIAN_POINT('',(-2.,5.,1.));
#21188=CARTESIAN_POINT('',(-2.,-5.,1.));
#21189=CARTESIAN_POINT('',(-2.,5.,1.));
#21190=CARTESIAN_POINT('Origin',(1.,5.,1.));
#21191=CARTESIAN_POINT('',(-1.,5.,8.5));
#21192=CARTESIAN_POINT('',(-1.,5.,1.));
#21193=CARTESIAN_POINT('',(1.,5.,8.5));
#21194=CARTESIAN_POINT('',(1.,5.,8.5));
#21195=CARTESIAN_POINT('',(1.,5.,1.));
#21196=CARTESIAN_POINT('',(2.,5.,1.));
#21197=CARTESIAN_POINT('',(-0.605,5.,3.));
#21198=CARTESIAN_POINT('Origin',(0.,5.,3.));
#21199=CARTESIAN_POINT('Origin',(-1.,5.,1.));
#21200=CARTESIAN_POINT('',(-1.,-5.,8.5));
#21201=CARTESIAN_POINT('',(-1.,-5.,1.));
#21202=CARTESIAN_POINT('',(-1.,5.,8.5));
#21203=CARTESIAN_POINT('',(-1.,-3.,6.605));
#21204=CARTESIAN_POINT('Origin',(-1.,-3.,6.));
#21205=CARTESIAN_POINT('',(-1.,3.,6.605));
#21206=CARTESIAN_POINT('Origin',(-1.,3.,6.));
#21207=CARTESIAN_POINT('Origin',(0.,-5.1,3.));
#21208=CARTESIAN_POINT('',(-0.605,-5.,3.));
#21209=CARTESIAN_POINT('Origin',(0.,-5.,3.));
#21210=CARTESIAN_POINT('',(-0.605,-5.1,3.));
#21211=CARTESIAN_POINT('Origin',(-1.1,-3.,6.));
#21212=CARTESIAN_POINT('',(1.,-3.,6.605));
#21213=CARTESIAN_POINT('',(-1.1,-3.,6.605));
#21214=CARTESIAN_POINT('Origin',(1.,-3.,6.));
#21215=CARTESIAN_POINT('Origin',(-1.1,3.,6.));
#21216=CARTESIAN_POINT('',(1.,3.,6.605));
#21217=CARTESIAN_POINT('',(-1.1,3.,6.605));
#21218=CARTESIAN_POINT('Origin',(1.,3.,6.));
#21219=CARTESIAN_POINT('Origin',(1.,-5.,1.));
#21220=CARTESIAN_POINT('',(1.,-5.,8.5));
#21221=CARTESIAN_POINT('',(1.,-5.,8.5));
#21222=CARTESIAN_POINT('',(1.,-5.,1.));
#21223=CARTESIAN_POINT('Origin',(-1.,-5.,1.));
#21224=CARTESIAN_POINT('',(-1.,-5.,8.5));
#21225=CARTESIAN_POINT('',(-2.,-5.,1.));
#21226=CARTESIAN_POINT('Origin',(0.,0.,8.5));
#21227=CARTESIAN_POINT('Origin',(0.,0.,1.));
#21228=CARTESIAN_POINT('',(0.,0.,0.));
#21229=CARTESIAN_POINT('Origin',(-1.4,-1.30814754519511,4.69185245480489));
#21230=CARTESIAN_POINT('',(-1.3,-1.30814754519511,4.91685245480489));
#21231=CARTESIAN_POINT('Origin',(-1.3,-1.30814754519511,4.69185245480489));
#21232=CARTESIAN_POINT('',(-1.,-1.30814754519511,4.91685245480489));
#21233=CARTESIAN_POINT('',(-1.4,-1.30814754519511,4.91685245480489));
#21234=CARTESIAN_POINT('Origin',(-1.,-1.30814754519511,4.69185245480489));
#21235=CARTESIAN_POINT('Origin',(-1.4,-1.30814754519511,7.30814754519511));
#21236=CARTESIAN_POINT('',(-1.3,-1.30814754519511,7.53314754519511));
#21237=CARTESIAN_POINT('Origin',(-1.3,-1.30814754519511,7.30814754519511));
#21238=CARTESIAN_POINT('',(-1.,-1.30814754519511,7.53314754519511));
#21239=CARTESIAN_POINT('',(-1.4,-1.30814754519511,7.53314754519511));
#21240=CARTESIAN_POINT('Origin',(-1.,-1.30814754519511,7.30814754519511));
#21241=CARTESIAN_POINT('Origin',(-1.4,1.30814754519511,7.30814754519511));
#21242=CARTESIAN_POINT('',(-1.3,1.30814754519511,7.53314754519511));
#21243=CARTESIAN_POINT('Origin',(-1.3,1.30814754519511,7.30814754519511));
#21244=CARTESIAN_POINT('',(-1.,1.30814754519511,7.53314754519511));
#21245=CARTESIAN_POINT('',(-1.4,1.30814754519511,7.53314754519511));
#21246=CARTESIAN_POINT('Origin',(-1.,1.30814754519511,7.30814754519511));
#21247=CARTESIAN_POINT('Origin',(-1.4,1.30814754519511,4.69185245480489));
#21248=CARTESIAN_POINT('',(-1.3,1.30814754519511,4.91685245480489));
#21249=CARTESIAN_POINT('Origin',(-1.3,1.30814754519511,4.69185245480489));
#21250=CARTESIAN_POINT('',(-1.,1.30814754519511,4.91685245480489));
#21251=CARTESIAN_POINT('',(-1.4,1.30814754519511,4.91685245480489));
#21252=CARTESIAN_POINT('Origin',(-1.,1.30814754519511,4.69185245480489));
#21253=CARTESIAN_POINT('Origin',(-1.,0.,6.));
#21254=CARTESIAN_POINT('',(-0.5,-1.94718841064429E-16,7.59));
#21255=CARTESIAN_POINT('Origin',(-0.5,0.,6.));
#21256=CARTESIAN_POINT('',(-1.,-1.94718841064429E-16,7.59));
#21257=CARTESIAN_POINT('',(-1.,-1.94718841064429E-16,7.59));
#21258=CARTESIAN_POINT('Origin',(-1.,0.,6.));
#21259=CARTESIAN_POINT('Origin',(-0.5,0.,6.));
#21260=CARTESIAN_POINT('',(-0.5,-1.2491397351303E-16,7.02));
#21261=CARTESIAN_POINT('Origin',(-0.5,0.,6.));
#21262=CARTESIAN_POINT('Origin',(-1.3,0.,6.));
#21263=CARTESIAN_POINT('',(-1.3,-1.2491397351303E-16,7.02));
#21264=CARTESIAN_POINT('',(-1.3,-1.2491397351303E-16,7.02));
#21265=CARTESIAN_POINT('Origin',(-1.3,0.,6.));
#21266=CARTESIAN_POINT('Origin',(-1.3,0.,6.));
#21267=CARTESIAN_POINT('',(-1.,-2.69422295812418E-16,8.2));
#21268=CARTESIAN_POINT('Origin',(-1.,0.,6.));
#21269=CARTESIAN_POINT('',(-1.3,-2.69422295812418E-16,8.2));
#21270=CARTESIAN_POINT('',(-1.3,-2.69422295812418E-16,8.2));
#21271=CARTESIAN_POINT('Origin',(-1.3,0.,6.));
#21272=CARTESIAN_POINT('Origin',(-1.,0.,6.));
#21273=CARTESIAN_POINT('Origin',(-1.3,0.,6.));
#21274=CARTESIAN_POINT('',(0.,0.,0.));
#21275=CARTESIAN_POINT('Origin',(0.9,-1.30814754519511,4.69185245480489));
#21276=CARTESIAN_POINT('',(1.,-1.30814754519511,4.91685245480489));
#21277=CARTESIAN_POINT('Origin',(1.,-1.30814754519511,4.69185245480489));
#21278=CARTESIAN_POINT('',(1.3,-1.30814754519511,4.91685245480489));
#21279=CARTESIAN_POINT('',(0.9,-1.30814754519511,4.91685245480489));
#21280=CARTESIAN_POINT('Origin',(1.3,-1.30814754519511,4.69185245480489));
#21281=CARTESIAN_POINT('Origin',(0.9,-1.30814754519511,7.30814754519511));
#21282=CARTESIAN_POINT('',(1.,-1.30814754519511,7.53314754519511));
#21283=CARTESIAN_POINT('Origin',(1.,-1.30814754519511,7.30814754519511));
#21284=CARTESIAN_POINT('',(1.3,-1.30814754519511,7.53314754519511));
#21285=CARTESIAN_POINT('',(0.9,-1.30814754519511,7.53314754519511));
#21286=CARTESIAN_POINT('Origin',(1.3,-1.30814754519511,7.30814754519511));
#21287=CARTESIAN_POINT('Origin',(0.9,1.30814754519511,7.30814754519511));
#21288=CARTESIAN_POINT('',(1.,1.30814754519511,7.53314754519511));
#21289=CARTESIAN_POINT('Origin',(1.,1.30814754519511,7.30814754519511));
#21290=CARTESIAN_POINT('',(1.3,1.30814754519511,7.53314754519511));
#21291=CARTESIAN_POINT('',(0.9,1.30814754519511,7.53314754519511));
#21292=CARTESIAN_POINT('Origin',(1.3,1.30814754519511,7.30814754519511));
#21293=CARTESIAN_POINT('Origin',(0.9,1.30814754519511,4.69185245480489));
#21294=CARTESIAN_POINT('',(1.,1.30814754519511,4.91685245480489));
#21295=CARTESIAN_POINT('Origin',(1.,1.30814754519511,4.69185245480489));
#21296=CARTESIAN_POINT('',(1.3,1.30814754519511,4.91685245480489));
#21297=CARTESIAN_POINT('',(0.9,1.30814754519511,4.91685245480489));
#21298=CARTESIAN_POINT('Origin',(1.3,1.30814754519511,4.69185245480489));
#21299=CARTESIAN_POINT('Origin',(0.5,0.,6.));
#21300=CARTESIAN_POINT('',(1.,-1.94718841064429E-16,7.59));
#21301=CARTESIAN_POINT('Origin',(1.,0.,6.));
#21302=CARTESIAN_POINT('',(0.5,-1.94718841064429E-16,7.59));
#21303=CARTESIAN_POINT('',(0.5,-1.94718841064429E-16,7.59));
#21304=CARTESIAN_POINT('Origin',(0.5,0.,6.));
#21305=CARTESIAN_POINT('Origin',(0.5,0.,6.));
#21306=CARTESIAN_POINT('',(0.5,-1.2491397351303E-16,7.02));
#21307=CARTESIAN_POINT('Origin',(0.5,0.,6.));
#21308=CARTESIAN_POINT('Origin',(1.,0.,6.));
#21309=CARTESIAN_POINT('',(1.3,-1.2491397351303E-16,7.02));
#21310=CARTESIAN_POINT('Origin',(1.3,0.,6.));
#21311=CARTESIAN_POINT('',(1.,-1.2491397351303E-16,7.02));
#21312=CARTESIAN_POINT('Origin',(1.,0.,6.));
#21313=CARTESIAN_POINT('',(1.3,-2.69422295812418E-16,8.2));
#21314=CARTESIAN_POINT('Origin',(1.3,0.,6.));
#21315=CARTESIAN_POINT('',(1.,-2.69422295812418E-16,8.2));
#21316=CARTESIAN_POINT('',(1.,-2.69422295812418E-16,8.2));
#21317=CARTESIAN_POINT('Origin',(1.,0.,6.));
#21318=CARTESIAN_POINT('Origin',(1.3,0.,6.));
#21319=CARTESIAN_POINT('Origin',(1.,0.,6.));
#21320=CARTESIAN_POINT('',(0.,0.,0.));
#21321=CARTESIAN_POINT('Origin',(43.9,-1.30814754519511,4.69185245480489));
#21322=CARTESIAN_POINT('',(44.,-1.30814754519511,4.85685245480489));
#21323=CARTESIAN_POINT('Origin',(44.,-1.30814754519511,4.69185245480489));
#21324=CARTESIAN_POINT('',(46.,-1.30814754519511,4.85685245480489));
#21325=CARTESIAN_POINT('',(43.9,-1.30814754519511,4.85685245480489));
#21326=CARTESIAN_POINT('Origin',(46.,-1.30814754519511,4.69185245480489));
#21327=CARTESIAN_POINT('Origin',(43.9,-1.30814754519511,7.30814754519511));
#21328=CARTESIAN_POINT('',(44.,-1.30814754519511,7.47314754519511));
#21329=CARTESIAN_POINT('Origin',(44.,-1.30814754519511,7.30814754519511));
#21330=CARTESIAN_POINT('',(46.,-1.30814754519511,7.47314754519511));
#21331=CARTESIAN_POINT('',(43.9,-1.30814754519511,7.47314754519511));
#21332=CARTESIAN_POINT('Origin',(46.,-1.30814754519511,7.30814754519511));
#21333=CARTESIAN_POINT('Origin',(43.9,1.30814754519511,7.30814754519511));
#21334=CARTESIAN_POINT('',(44.,1.30814754519511,7.47314754519511));
#21335=CARTESIAN_POINT('Origin',(44.,1.30814754519511,7.30814754519511));
#21336=CARTESIAN_POINT('',(46.,1.30814754519511,7.47314754519511));
#21337=CARTESIAN_POINT('',(43.9,1.30814754519511,7.47314754519511));
#21338=CARTESIAN_POINT('Origin',(46.,1.30814754519511,7.30814754519511));
#21339=CARTESIAN_POINT('Origin',(43.9,1.30814754519511,4.69185245480489));
#21340=CARTESIAN_POINT('',(44.,1.30814754519511,4.85685245480489));
#21341=CARTESIAN_POINT('Origin',(44.,1.30814754519511,4.69185245480489));
#21342=CARTESIAN_POINT('',(46.,1.30814754519511,4.85685245480489));
#21343=CARTESIAN_POINT('',(43.9,1.30814754519511,4.85685245480489));
#21344=CARTESIAN_POINT('Origin',(46.,1.30814754519511,4.69185245480489));
#21345=CARTESIAN_POINT('Origin',(43.9,0.,6.));
#21346=CARTESIAN_POINT('',(44.,-1.95943487863576E-16,7.6));
#21347=CARTESIAN_POINT('Origin',(44.,0.,6.));
#21348=CARTESIAN_POINT('',(46.,1.95943487863576E-16,7.6));
#21349=CARTESIAN_POINT('',(43.9,-1.95943487863576E-16,7.6));
#21350=CARTESIAN_POINT('Origin',(46.,0.,6.));
#21351=CARTESIAN_POINT('Origin',(46.5,-4.,0.9));
#21352=CARTESIAN_POINT('',(46.225,-4.,1.));
#21353=CARTESIAN_POINT('Origin',(46.5,-4.,1.));
#21354=CARTESIAN_POINT('',(46.225,-4.,2.));
#21355=CARTESIAN_POINT('',(46.225,-4.,0.9));
#21356=CARTESIAN_POINT('Origin',(46.5,-4.,2.));
#21357=CARTESIAN_POINT('Origin',(43.5,4.,0.9));
#21358=CARTESIAN_POINT('',(43.225,4.,1.));
#21359=CARTESIAN_POINT('Origin',(43.5,4.,1.));
#21360=CARTESIAN_POINT('',(43.225,4.,2.));
#21361=CARTESIAN_POINT('',(43.225,4.,0.9));
#21362=CARTESIAN_POINT('Origin',(43.5,4.,2.));
#21363=CARTESIAN_POINT('Origin',(43.5,-4.,0.9));
#21364=CARTESIAN_POINT('',(43.225,-4.,1.));
#21365=CARTESIAN_POINT('Origin',(43.5,-4.,1.));
#21366=CARTESIAN_POINT('',(43.225,-4.,2.));
#21367=CARTESIAN_POINT('',(43.225,-4.,0.9));
#21368=CARTESIAN_POINT('Origin',(43.5,-4.,2.));
#21369=CARTESIAN_POINT('Origin',(46.5,4.,0.9));
#21370=CARTESIAN_POINT('',(46.225,4.,1.));
#21371=CARTESIAN_POINT('Origin',(46.5,4.,1.));
#21372=CARTESIAN_POINT('',(46.225,4.,2.));
#21373=CARTESIAN_POINT('',(46.225,4.,0.9));
#21374=CARTESIAN_POINT('Origin',(46.5,4.,2.));
#21375=CARTESIAN_POINT('Origin',(45.,0.,2.));
#21376=CARTESIAN_POINT('',(44.,5.,2.));
#21377=CARTESIAN_POINT('',(44.,-5.,2.));
#21378=CARTESIAN_POINT('',(44.,2.5,2.));
#21379=CARTESIAN_POINT('',(43.,5.,2.));
#21380=CARTESIAN_POINT('',(47.,5.,2.));
#21381=CARTESIAN_POINT('',(43.,-5.,2.));
#21382=CARTESIAN_POINT('',(43.,5.,2.));
#21383=CARTESIAN_POINT('',(43.,-5.,2.));
#21384=CARTESIAN_POINT('Origin',(45.,0.,2.));
#21385=CARTESIAN_POINT('',(46.,-5.,2.));
#21386=CARTESIAN_POINT('',(46.,5.,2.));
#21387=CARTESIAN_POINT('',(46.,-2.5,2.));
#21388=CARTESIAN_POINT('',(47.,-5.,2.));
#21389=CARTESIAN_POINT('',(43.,-5.,2.));
#21390=CARTESIAN_POINT('',(47.,5.,2.));
#21391=CARTESIAN_POINT('',(47.,-5.,2.));
#21392=CARTESIAN_POINT('',(47.,5.,2.));
#21393=CARTESIAN_POINT('Origin',(47.,-5.,1.));
#21394=CARTESIAN_POINT('',(47.,-5.,1.));
#21395=CARTESIAN_POINT('',(47.,5.,1.));
#21396=CARTESIAN_POINT('',(47.,-5.,1.));
#21397=CARTESIAN_POINT('',(47.,5.,1.));
#21398=CARTESIAN_POINT('',(47.,-5.,1.));
#21399=CARTESIAN_POINT('Origin',(43.,5.,1.));
#21400=CARTESIAN_POINT('',(43.,5.,1.));
#21401=CARTESIAN_POINT('',(43.,-5.,1.));
#21402=CARTESIAN_POINT('',(43.,5.,1.));
#21403=CARTESIAN_POINT('',(43.,-5.,1.));
#21404=CARTESIAN_POINT('',(43.,5.,1.));
#21405=CARTESIAN_POINT('Origin',(46.,5.,1.));
#21406=CARTESIAN_POINT('',(44.,5.,8.5));
#21407=CARTESIAN_POINT('',(44.,5.,1.));
#21408=CARTESIAN_POINT('',(46.,5.,8.5));
#21409=CARTESIAN_POINT('',(46.,5.,8.5));
#21410=CARTESIAN_POINT('',(46.,5.,1.));
#21411=CARTESIAN_POINT('',(47.,5.,1.));
#21412=CARTESIAN_POINT('Origin',(44.,5.,1.));
#21413=CARTESIAN_POINT('',(44.,-5.,8.5));
#21414=CARTESIAN_POINT('',(44.,-5.,1.));
#21415=CARTESIAN_POINT('',(44.,5.,8.5));
#21416=CARTESIAN_POINT('',(44.,-3.,6.605));
#21417=CARTESIAN_POINT('Origin',(44.,-3.,6.));
#21418=CARTESIAN_POINT('',(44.,3.,6.605));
#21419=CARTESIAN_POINT('Origin',(44.,3.,6.));
#21420=CARTESIAN_POINT('Origin',(43.9,-3.,6.));
#21421=CARTESIAN_POINT('',(46.,-3.,6.605));
#21422=CARTESIAN_POINT('',(43.9,-3.,6.605));
#21423=CARTESIAN_POINT('Origin',(46.,-3.,6.));
#21424=CARTESIAN_POINT('Origin',(43.9,3.,6.));
#21425=CARTESIAN_POINT('',(46.,3.,6.605));
#21426=CARTESIAN_POINT('',(43.9,3.,6.605));
#21427=CARTESIAN_POINT('Origin',(46.,3.,6.));
#21428=CARTESIAN_POINT('Origin',(46.,-5.,1.));
#21429=CARTESIAN_POINT('',(46.,-5.,8.5));
#21430=CARTESIAN_POINT('',(46.,-5.,8.5));
#21431=CARTESIAN_POINT('',(46.,-5.,1.));
#21432=CARTESIAN_POINT('Origin',(44.,-5.,1.));
#21433=CARTESIAN_POINT('',(44.,-5.,8.5));
#21434=CARTESIAN_POINT('',(43.,-5.,1.));
#21435=CARTESIAN_POINT('Origin',(45.,0.,8.5));
#21436=CARTESIAN_POINT('Origin',(45.,0.,1.));
#21437=CARTESIAN_POINT('',(0.,0.,0.));
#21438=CARTESIAN_POINT('Origin',(43.6,-1.30814754519511,4.69185245480489));
#21439=CARTESIAN_POINT('',(43.7,-1.30814754519511,4.91685245480489));
#21440=CARTESIAN_POINT('Origin',(43.7,-1.30814754519511,4.69185245480489));
#21441=CARTESIAN_POINT('',(44.,-1.30814754519511,4.91685245480489));
#21442=CARTESIAN_POINT('',(43.6,-1.30814754519511,4.91685245480489));
#21443=CARTESIAN_POINT('Origin',(44.,-1.30814754519511,4.69185245480489));
#21444=CARTESIAN_POINT('Origin',(43.6,-1.30814754519511,7.30814754519511));
#21445=CARTESIAN_POINT('',(43.7,-1.30814754519511,7.53314754519511));
#21446=CARTESIAN_POINT('Origin',(43.7,-1.30814754519511,7.30814754519511));
#21447=CARTESIAN_POINT('',(44.,-1.30814754519511,7.53314754519511));
#21448=CARTESIAN_POINT('',(43.6,-1.30814754519511,7.53314754519511));
#21449=CARTESIAN_POINT('Origin',(44.,-1.30814754519511,7.30814754519511));
#21450=CARTESIAN_POINT('Origin',(43.6,1.30814754519511,7.30814754519511));
#21451=CARTESIAN_POINT('',(43.7,1.30814754519511,7.53314754519511));
#21452=CARTESIAN_POINT('Origin',(43.7,1.30814754519511,7.30814754519511));
#21453=CARTESIAN_POINT('',(44.,1.30814754519511,7.53314754519511));
#21454=CARTESIAN_POINT('',(43.6,1.30814754519511,7.53314754519511));
#21455=CARTESIAN_POINT('Origin',(44.,1.30814754519511,7.30814754519511));
#21456=CARTESIAN_POINT('Origin',(43.6,1.30814754519511,4.69185245480489));
#21457=CARTESIAN_POINT('',(43.7,1.30814754519511,4.91685245480489));
#21458=CARTESIAN_POINT('Origin',(43.7,1.30814754519511,4.69185245480489));
#21459=CARTESIAN_POINT('',(44.,1.30814754519511,4.91685245480489));
#21460=CARTESIAN_POINT('',(43.6,1.30814754519511,4.91685245480489));
#21461=CARTESIAN_POINT('Origin',(44.,1.30814754519511,4.69185245480489));
#21462=CARTESIAN_POINT('Origin',(44.,0.,6.));
#21463=CARTESIAN_POINT('',(44.5,-1.94718841064429E-16,7.59));
#21464=CARTESIAN_POINT('Origin',(44.5,0.,6.));
#21465=CARTESIAN_POINT('',(44.,-1.94718841064429E-16,7.59));
#21466=CARTESIAN_POINT('',(44.,-1.94718841064429E-16,7.59));
#21467=CARTESIAN_POINT('Origin',(44.,0.,6.));
#21468=CARTESIAN_POINT('Origin',(44.5,0.,6.));
#21469=CARTESIAN_POINT('',(44.5,-1.2491397351303E-16,7.02));
#21470=CARTESIAN_POINT('Origin',(44.5,0.,6.));
#21471=CARTESIAN_POINT('Origin',(43.7,0.,6.));
#21472=CARTESIAN_POINT('',(43.7,-1.2491397351303E-16,7.02));
#21473=CARTESIAN_POINT('',(43.7,-1.2491397351303E-16,7.02));
#21474=CARTESIAN_POINT('Origin',(43.7,0.,6.));
#21475=CARTESIAN_POINT('Origin',(43.7,0.,6.));
#21476=CARTESIAN_POINT('',(44.,-2.69422295812418E-16,8.2));
#21477=CARTESIAN_POINT('Origin',(44.,0.,6.));
#21478=CARTESIAN_POINT('',(43.7,-2.69422295812418E-16,8.2));
#21479=CARTESIAN_POINT('',(43.7,-2.69422295812418E-16,8.2));
#21480=CARTESIAN_POINT('Origin',(43.7,0.,6.));
#21481=CARTESIAN_POINT('Origin',(44.,0.,6.));
#21482=CARTESIAN_POINT('Origin',(43.7,0.,6.));
#21483=CARTESIAN_POINT('',(0.,0.,0.));
#21484=CARTESIAN_POINT('Origin',(45.9,-1.30814754519511,4.69185245480489));
#21485=CARTESIAN_POINT('',(46.,-1.30814754519511,4.91685245480489));
#21486=CARTESIAN_POINT('Origin',(46.,-1.30814754519511,4.69185245480489));
#21487=CARTESIAN_POINT('',(46.3,-1.30814754519511,4.91685245480489));
#21488=CARTESIAN_POINT('',(45.9,-1.30814754519511,4.91685245480489));
#21489=CARTESIAN_POINT('Origin',(46.3,-1.30814754519511,4.69185245480489));
#21490=CARTESIAN_POINT('Origin',(45.9,-1.30814754519511,7.30814754519511));
#21491=CARTESIAN_POINT('',(46.,-1.30814754519511,7.53314754519511));
#21492=CARTESIAN_POINT('Origin',(46.,-1.30814754519511,7.30814754519511));
#21493=CARTESIAN_POINT('',(46.3,-1.30814754519511,7.53314754519511));
#21494=CARTESIAN_POINT('',(45.9,-1.30814754519511,7.53314754519511));
#21495=CARTESIAN_POINT('Origin',(46.3,-1.30814754519511,7.30814754519511));
#21496=CARTESIAN_POINT('Origin',(45.9,1.30814754519511,7.30814754519511));
#21497=CARTESIAN_POINT('',(46.,1.30814754519511,7.53314754519511));
#21498=CARTESIAN_POINT('Origin',(46.,1.30814754519511,7.30814754519511));
#21499=CARTESIAN_POINT('',(46.3,1.30814754519511,7.53314754519511));
#21500=CARTESIAN_POINT('',(45.9,1.30814754519511,7.53314754519511));
#21501=CARTESIAN_POINT('Origin',(46.3,1.30814754519511,7.30814754519511));
#21502=CARTESIAN_POINT('Origin',(45.9,1.30814754519511,4.69185245480489));
#21503=CARTESIAN_POINT('',(46.,1.30814754519511,4.91685245480489));
#21504=CARTESIAN_POINT('Origin',(46.,1.30814754519511,4.69185245480489));
#21505=CARTESIAN_POINT('',(46.3,1.30814754519511,4.91685245480489));
#21506=CARTESIAN_POINT('',(45.9,1.30814754519511,4.91685245480489));
#21507=CARTESIAN_POINT('Origin',(46.3,1.30814754519511,4.69185245480489));
#21508=CARTESIAN_POINT('Origin',(45.5,0.,6.));
#21509=CARTESIAN_POINT('',(46.,-1.94718841064429E-16,7.59));
#21510=CARTESIAN_POINT('Origin',(46.,0.,6.));
#21511=CARTESIAN_POINT('',(45.5,-1.94718841064429E-16,7.59));
#21512=CARTESIAN_POINT('',(45.5,-1.94718841064429E-16,7.59));
#21513=CARTESIAN_POINT('Origin',(45.5,0.,6.));
#21514=CARTESIAN_POINT('Origin',(45.5,0.,6.));
#21515=CARTESIAN_POINT('',(45.5,-1.2491397351303E-16,7.02));
#21516=CARTESIAN_POINT('Origin',(45.5,0.,6.));
#21517=CARTESIAN_POINT('Origin',(46.,0.,6.));
#21518=CARTESIAN_POINT('',(46.3,-1.2491397351303E-16,7.02));
#21519=CARTESIAN_POINT('Origin',(46.3,0.,6.));
#21520=CARTESIAN_POINT('',(46.,-1.2491397351303E-16,7.02));
#21521=CARTESIAN_POINT('Origin',(46.,0.,6.));
#21522=CARTESIAN_POINT('',(46.3,-2.69422295812418E-16,8.2));
#21523=CARTESIAN_POINT('Origin',(46.3,0.,6.));
#21524=CARTESIAN_POINT('',(46.,-2.69422295812418E-16,8.2));
#21525=CARTESIAN_POINT('',(46.,-2.69422295812418E-16,8.2));
#21526=CARTESIAN_POINT('Origin',(46.,0.,6.));
#21527=CARTESIAN_POINT('Origin',(46.3,0.,6.));
#21528=CARTESIAN_POINT('Origin',(46.,0.,6.));
#21529=CARTESIAN_POINT('',(0.,0.,0.));
#21530=CARTESIAN_POINT('Origin',(-1.,-3.,6.));
#21531=CARTESIAN_POINT('',(47.,-3.,6.6));
#21532=CARTESIAN_POINT('Origin',(47.,-3.,6.));
#21533=CARTESIAN_POINT('',(-1.,-3.,6.6));
#21534=CARTESIAN_POINT('',(-1.,-3.,6.6));
#21535=CARTESIAN_POINT('Origin',(-1.,-3.,6.));
#21536=CARTESIAN_POINT('Origin',(47.,-3.,6.));
#21537=CARTESIAN_POINT('Origin',(-1.,-3.,6.));
#21538=CARTESIAN_POINT('',(0.,0.,0.));
#21539=CARTESIAN_POINT('Origin',(-1.,3.,6.));
#21540=CARTESIAN_POINT('',(47.,3.,6.6));
#21541=CARTESIAN_POINT('Origin',(47.,3.,6.));
#21542=CARTESIAN_POINT('',(-1.,3.,6.6));
#21543=CARTESIAN_POINT('',(-1.,3.,6.6));
#21544=CARTESIAN_POINT('Origin',(-1.,3.,6.));
#21545=CARTESIAN_POINT('Origin',(47.,3.,6.));
#21546=CARTESIAN_POINT('Origin',(-1.,3.,6.));
#21547=CARTESIAN_POINT('',(0.,0.,0.));
#21548=CARTESIAN_POINT('Origin',(0.,4.9,3.));
#21549=CARTESIAN_POINT('',(-0.165,4.9,3.));
#21550=CARTESIAN_POINT('Origin',(0.,4.9,3.));
#21551=CARTESIAN_POINT('',(-0.165,6.5,3.));
#21552=CARTESIAN_POINT('',(-0.165,4.9,3.));
#21553=CARTESIAN_POINT('Origin',(0.,6.5,3.));
#21554=CARTESIAN_POINT('Origin',(0.,4.9,3.));
#21555=CARTESIAN_POINT('Origin',(0.,-7.6,3.));
#21556=CARTESIAN_POINT('',(-0.165,-7.5,3.));
#21557=CARTESIAN_POINT('Origin',(0.,-7.5,3.));
#21558=CARTESIAN_POINT('',(-0.165,-5.9,3.));
#21559=CARTESIAN_POINT('',(-0.165,-7.6,3.));
#21560=CARTESIAN_POINT('Origin',(0.,-5.9,3.));
#21561=CARTESIAN_POINT('Origin',(0.,-5.9,3.));
#21562=CARTESIAN_POINT('Origin',(0.,-7.5,3.));
#21563=CARTESIAN_POINT('',(-0.6,6.5,3.));
#21564=CARTESIAN_POINT('Origin',(0.,6.5,3.));
#21565=CARTESIAN_POINT('',(-0.6,-7.5,3.));
#21566=CARTESIAN_POINT('',(-0.6,-7.5,3.));
#21567=CARTESIAN_POINT('Origin',(0.,-7.5,3.));
#21568=CARTESIAN_POINT('Origin',(0.,6.5,3.));
#21569=CARTESIAN_POINT('Origin',(0.,-7.5,3.));
#21570=CARTESIAN_POINT('',(0.,0.,0.));
#21571=CARTESIAN_POINT('Origin',(0.,-7.7,3.));
#21572=CARTESIAN_POINT('',(-0.225,-7.5,3.));
#21573=CARTESIAN_POINT('Origin',(0.,-7.5,3.));
#21574=CARTESIAN_POINT('',(-0.225,-7.7,3.));
#21575=CARTESIAN_POINT('',(-0.225,-7.7,3.));
#21576=CARTESIAN_POINT('Origin',(0.,-7.7,3.));
#21577=CARTESIAN_POINT('Origin',(0.,-7.7,3.));
#21578=CARTESIAN_POINT('',(-1.,-7.5,3.));
#21579=CARTESIAN_POINT('Origin',(0.,-7.5,3.));
#21580=CARTESIAN_POINT('',(-1.,-7.7,3.));
#21581=CARTESIAN_POINT('',(-1.,-7.7,3.));
#21582=CARTESIAN_POINT('Origin',(0.,-7.7,3.));
#21583=CARTESIAN_POINT('Origin',(0.,-7.5,3.));
#21584=CARTESIAN_POINT('Origin',(0.,-7.7,3.));
#21585=CARTESIAN_POINT('',(0.,0.,0.));
#21586=CARTESIAN_POINT('Origin',(0.,6.5,3.));
#21587=CARTESIAN_POINT('',(-0.225,6.7,3.));
#21588=CARTESIAN_POINT('Origin',(0.,6.7,3.));
#21589=CARTESIAN_POINT('',(-0.225,6.5,3.));
#21590=CARTESIAN_POINT('',(-0.225,6.5,3.));
#21591=CARTESIAN_POINT('Origin',(0.,6.5,3.));
#21592=CARTESIAN_POINT('Origin',(0.,6.5,3.));
#21593=CARTESIAN_POINT('',(-1.,6.7,3.));
#21594=CARTESIAN_POINT('Origin',(0.,6.7,3.));
#21595=CARTESIAN_POINT('',(-1.,6.5,3.));
#21596=CARTESIAN_POINT('',(-1.,6.5,3.));
#21597=CARTESIAN_POINT('Origin',(0.,6.5,3.));
#21598=CARTESIAN_POINT('Origin',(0.,6.7,3.));
#21599=CARTESIAN_POINT('Origin',(0.,6.5,3.));
#21600=CARTESIAN_POINT('',(0.,0.,0.));
#21601=CARTESIAN_POINT('Origin',(0.,-7.5,3.));
#21602=CARTESIAN_POINT('',(-0.605,-7.,3.));
#21603=CARTESIAN_POINT('Origin',(0.,-7.,3.));
#21604=CARTESIAN_POINT('',(-0.605,-7.5,3.));
#21605=CARTESIAN_POINT('',(-0.605,-7.5,3.));
#21606=CARTESIAN_POINT('Origin',(0.,-7.5,3.));
#21607=CARTESIAN_POINT('Origin',(0.,-7.5,3.));
#21608=CARTESIAN_POINT('',(-0.8,-7.,3.));
#21609=CARTESIAN_POINT('Origin',(0.,-7.,3.));
#21610=CARTESIAN_POINT('',(-0.8,-7.5,3.));
#21611=CARTESIAN_POINT('',(-0.8,-7.5,3.));
#21612=CARTESIAN_POINT('Origin',(0.,-7.5,3.));
#21613=CARTESIAN_POINT('Origin',(0.,-7.,3.));
#21614=CARTESIAN_POINT('Origin',(0.,-7.5,3.));
#21615=CARTESIAN_POINT('',(0.,0.,0.));
#21616=CARTESIAN_POINT('Origin',(0.,-6.,3.));
#21617=CARTESIAN_POINT('',(-0.605,-5.,3.));
#21618=CARTESIAN_POINT('Origin',(0.,-5.,3.));
#21619=CARTESIAN_POINT('',(-0.605,-6.,3.));
#21620=CARTESIAN_POINT('',(-0.605,-6.,3.));
#21621=CARTESIAN_POINT('Origin',(0.,-6.,3.));
#21622=CARTESIAN_POINT('Origin',(0.,-6.,3.));
#21623=CARTESIAN_POINT('',(-0.8,-5.,3.));
#21624=CARTESIAN_POINT('Origin',(0.,-5.,3.));
#21625=CARTESIAN_POINT('',(-0.8,-6.,3.));
#21626=CARTESIAN_POINT('',(-0.8,-6.,3.));
#21627=CARTESIAN_POINT('Origin',(0.,-6.,3.));
#21628=CARTESIAN_POINT('Origin',(0.,-5.,3.));
#21629=CARTESIAN_POINT('Origin',(0.,-6.,3.));
#21630=CARTESIAN_POINT('',(0.,0.,0.));
#21631=CARTESIAN_POINT('Origin',(0.,6.,3.));
#21632=CARTESIAN_POINT('',(-0.605,6.5,3.));
#21633=CARTESIAN_POINT('Origin',(0.,6.5,3.));
#21634=CARTESIAN_POINT('',(-0.605,6.,3.));
#21635=CARTESIAN_POINT('',(-0.605,6.,3.));
#21636=CARTESIAN_POINT('Origin',(0.,6.,3.));
#21637=CARTESIAN_POINT('Origin',(0.,6.,3.));
#21638=CARTESIAN_POINT('',(-0.8,6.5,3.));
#21639=CARTESIAN_POINT('Origin',(0.,6.5,3.));
#21640=CARTESIAN_POINT('',(-0.8,6.,3.));
#21641=CARTESIAN_POINT('',(-0.8,6.,3.));
#21642=CARTESIAN_POINT('Origin',(0.,6.,3.));
#21643=CARTESIAN_POINT('Origin',(0.,6.5,3.));
#21644=CARTESIAN_POINT('Origin',(0.,6.,3.));
#21645=CARTESIAN_POINT('',(0.,0.,0.));
#21646=CARTESIAN_POINT('Origin',(0.0866025403784439,-0.4,-0.15));
#21647=CARTESIAN_POINT('',(0.173205080756888,-0.4,0.));
#21648=CARTESIAN_POINT('',(0.0866025403784439,-0.4,-0.15));
#21649=CARTESIAN_POINT('',(0.173205080756888,-0.4,0.));
#21650=CARTESIAN_POINT('',(0.0866025403784439,-0.64,-0.15));
#21651=CARTESIAN_POINT('',(0.0866025403784439,-0.4,-0.15));
#21652=CARTESIAN_POINT('',(0.173205080756888,-0.64,0.));
#21653=CARTESIAN_POINT('',(0.173205080756888,-0.64,0.));
#21654=CARTESIAN_POINT('',(0.173205080756888,-0.4,0.));
#21655=CARTESIAN_POINT('Origin',(-0.0866025403784438,-0.4,-0.15));
#21656=CARTESIAN_POINT('',(-0.0866025403784438,-0.4,-0.15));
#21657=CARTESIAN_POINT('',(0.0866025403784439,-0.4,-0.15));
#21658=CARTESIAN_POINT('',(-0.0866025403784438,-0.64,-0.15));
#21659=CARTESIAN_POINT('',(-0.0866025403784438,-0.4,-0.15));
#21660=CARTESIAN_POINT('',(0.0866025403784439,-0.64,-0.15));
#21661=CARTESIAN_POINT('Origin',(-0.173205080756888,-0.4,-2.77555756156289E-17));
#21662=CARTESIAN_POINT('',(-0.173205080756888,-0.4,-2.12115047744981E-17));
#21663=CARTESIAN_POINT('',(-0.0866025403784438,-0.4,-0.15));
#21664=CARTESIAN_POINT('',(-0.173205080756888,-0.64,-2.77555756156289E-17));
#21665=CARTESIAN_POINT('',(-0.173205080756888,-0.4,-2.12115047744981E-17));
#21666=CARTESIAN_POINT('',(-0.0866025403784438,-0.64,-0.15));
#21667=CARTESIAN_POINT('Origin',(-0.0866025403784439,-0.4,0.15));
#21668=CARTESIAN_POINT('',(-0.0866025403784439,-0.4,0.15));
#21669=CARTESIAN_POINT('',(-0.173205080756888,-0.4,-2.12115047744981E-17));
#21670=CARTESIAN_POINT('',(-0.0866025403784439,-0.64,0.15));
#21671=CARTESIAN_POINT('',(-0.0866025403784439,-0.4,0.15));
#21672=CARTESIAN_POINT('',(-0.173205080756888,-0.64,-2.12115047744981E-17));
#21673=CARTESIAN_POINT('Origin',(0.0866025403784439,-0.4,0.15));
#21674=CARTESIAN_POINT('',(0.0866025403784439,-0.4,0.15));
#21675=CARTESIAN_POINT('',(-0.0866025403784439,-0.4,0.15));
#21676=CARTESIAN_POINT('',(0.0866025403784439,-0.64,0.15));
#21677=CARTESIAN_POINT('',(0.0866025403784439,-0.4,0.15));
#21678=CARTESIAN_POINT('',(-0.0866025403784439,-0.64,0.15));
#21679=CARTESIAN_POINT('Origin',(0.173205080756888,-0.4,0.));
#21680=CARTESIAN_POINT('',(0.0866025403784439,-0.4,0.15));
#21681=CARTESIAN_POINT('',(0.0866025403784439,-0.64,0.15));
#21682=CARTESIAN_POINT('Origin',(0.,-0.4,-2.77555756156289E-17));
#21683=CARTESIAN_POINT('Origin',(0.,-0.64,-2.77555756156289E-17));
#21684=CARTESIAN_POINT('Origin',(0.,-1.,0.));
#21685=CARTESIAN_POINT('',(-0.1954,-1.,2.39295984553393E-17));
#21686=CARTESIAN_POINT('Origin',(0.,-1.,0.));
#21687=CARTESIAN_POINT('Origin',(0.3,0.4,0.));
#21688=CARTESIAN_POINT('',(-0.3,0.4,-3.67394039744206E-17));
#21689=CARTESIAN_POINT('Origin',(0.,0.4,0.));
#21690=CARTESIAN_POINT('Origin',(0.,0.375,0.));
#21691=CARTESIAN_POINT('',(-0.35,0.35,-4.28626379701573E-17));
#21692=CARTESIAN_POINT('Origin',(0.,0.35,0.));
#21693=CARTESIAN_POINT('',(-0.325,0.375,-3.9801020972289E-17));
#21694=CARTESIAN_POINT('Origin',(0.,0.19,0.));
#21695=CARTESIAN_POINT('',(-0.35,0.03,-4.28626379701574E-17));
#21696=CARTESIAN_POINT('Origin',(0.,0.03,0.));
#21697=CARTESIAN_POINT('',(-0.35,0.19,-4.28626379701574E-17));
#21698=CARTESIAN_POINT('Origin',(0.,0.0149999999999999,0.));
#21699=CARTESIAN_POINT('',(-0.32,-3.29597460435593E-17,-3.91886975727153E-17));
#21700=CARTESIAN_POINT('Origin',(0.,0.,0.));
#21701=CARTESIAN_POINT('',(-0.335,0.0149999999999999,-4.10256677714363E-17));
#21702=CARTESIAN_POINT('Origin',(0.22,0.,0.));
#21703=CARTESIAN_POINT('',(-0.22,-6.93889390390723E-18,-2.69422295812418E-17));
#21704=CARTESIAN_POINT('Origin',(0.,0.,0.));
#21705=CARTESIAN_POINT('Origin',(0.,-0.02,0.));
#21706=CARTESIAN_POINT('',(-0.1954,-0.0492,2.39295984553393E-17));
#21707=CARTESIAN_POINT('Origin',(0.,-0.0492,0.));
#21708=CARTESIAN_POINT('',(-0.21,-0.02,-2.57175827820944E-17));
#21709=CARTESIAN_POINT('Origin',(0.,-0.8,0.));
#21710=CARTESIAN_POINT('',(-0.1954,-0.8,-2.39295984553393E-17));
#21711=CARTESIAN_POINT('',(0.,0.,0.));
#21712=CARTESIAN_POINT('',(0.,0.,0.));
#21713=CARTESIAN_POINT('Origin',(46.5,-4.,17.9));
#21714=CARTESIAN_POINT('',(46.225,-4.,18.));
#21715=CARTESIAN_POINT('Origin',(46.5,-4.,18.));
#21716=CARTESIAN_POINT('',(46.225,-4.,19.));
#21717=CARTESIAN_POINT('',(46.225,-4.,17.9));
#21718=CARTESIAN_POINT('Origin',(46.5,-4.,19.));
#21719=CARTESIAN_POINT('Origin',(43.5,4.,17.9));
#21720=CARTESIAN_POINT('',(43.225,4.,18.));
#21721=CARTESIAN_POINT('Origin',(43.5,4.,18.));
#21722=CARTESIAN_POINT('',(43.225,4.,19.));
#21723=CARTESIAN_POINT('',(43.225,4.,17.9));
#21724=CARTESIAN_POINT('Origin',(43.5,4.,19.));
#21725=CARTESIAN_POINT('Origin',(43.5,-4.,17.9));
#21726=CARTESIAN_POINT('',(43.225,-4.,18.));
#21727=CARTESIAN_POINT('Origin',(43.5,-4.,18.));
#21728=CARTESIAN_POINT('',(43.225,-4.,19.));
#21729=CARTESIAN_POINT('',(43.225,-4.,17.9));
#21730=CARTESIAN_POINT('Origin',(43.5,-4.,19.));
#21731=CARTESIAN_POINT('Origin',(46.5,4.,17.9));
#21732=CARTESIAN_POINT('',(46.225,4.,18.));
#21733=CARTESIAN_POINT('Origin',(46.5,4.,18.));
#21734=CARTESIAN_POINT('',(46.225,4.,19.));
#21735=CARTESIAN_POINT('',(46.225,4.,17.9));
#21736=CARTESIAN_POINT('Origin',(46.5,4.,19.));
#21737=CARTESIAN_POINT('Origin',(1.5,-4.,17.9));
#21738=CARTESIAN_POINT('',(1.225,-4.,18.));
#21739=CARTESIAN_POINT('Origin',(1.5,-4.,18.));
#21740=CARTESIAN_POINT('',(1.225,-4.,19.));
#21741=CARTESIAN_POINT('',(1.225,-4.,17.9));
#21742=CARTESIAN_POINT('Origin',(1.5,-4.,19.));
#21743=CARTESIAN_POINT('Origin',(-1.5,4.,17.9));
#21744=CARTESIAN_POINT('',(-1.775,4.,18.));
#21745=CARTESIAN_POINT('Origin',(-1.5,4.,18.));
#21746=CARTESIAN_POINT('',(-1.775,4.,19.));
#21747=CARTESIAN_POINT('',(-1.775,4.,17.9));
#21748=CARTESIAN_POINT('Origin',(-1.5,4.,19.));
#21749=CARTESIAN_POINT('Origin',(-1.5,-4.,17.9));
#21750=CARTESIAN_POINT('',(-1.775,-4.,18.));
#21751=CARTESIAN_POINT('Origin',(-1.5,-4.,18.));
#21752=CARTESIAN_POINT('',(-1.775,-4.,19.));
#21753=CARTESIAN_POINT('',(-1.775,-4.,17.9));
#21754=CARTESIAN_POINT('Origin',(-1.5,-4.,19.));
#21755=CARTESIAN_POINT('Origin',(1.5,4.,17.9));
#21756=CARTESIAN_POINT('',(1.225,4.,18.));
#21757=CARTESIAN_POINT('Origin',(1.5,4.,18.));
#21758=CARTESIAN_POINT('',(1.225,4.,19.));
#21759=CARTESIAN_POINT('',(1.225,4.,17.9));
#21760=CARTESIAN_POINT('Origin',(1.5,4.,19.));
#21761=CARTESIAN_POINT('Origin',(48.,10.,18.));
#21762=CARTESIAN_POINT('',(48.,10.,18.));
#21763=CARTESIAN_POINT('',(-3.,10.,18.));
#21764=CARTESIAN_POINT('',(48.,10.,18.));
#21765=CARTESIAN_POINT('',(-3.,10.,19.));
#21766=CARTESIAN_POINT('',(-3.,10.,18.));
#21767=CARTESIAN_POINT('',(48.,10.,19.));
#21768=CARTESIAN_POINT('',(48.,10.,19.));
#21769=CARTESIAN_POINT('',(48.,10.,18.));
#21770=CARTESIAN_POINT('Origin',(48.,-10.,18.));
#21771=CARTESIAN_POINT('',(48.,-10.,18.));
#21772=CARTESIAN_POINT('',(48.,-10.,18.));
#21773=CARTESIAN_POINT('',(48.,-10.,19.));
#21774=CARTESIAN_POINT('',(48.,-10.,19.));
#21775=CARTESIAN_POINT('',(48.,-10.,18.));
#21776=CARTESIAN_POINT('Origin',(-3.,-10.,18.));
#21777=CARTESIAN_POINT('',(-3.,-10.,18.));
#21778=CARTESIAN_POINT('',(-3.,-10.,18.));
#21779=CARTESIAN_POINT('',(-3.,-10.,19.));
#21780=CARTESIAN_POINT('',(-3.,-10.,19.));
#21781=CARTESIAN_POINT('',(-3.,-10.,18.));
#21782=CARTESIAN_POINT('Origin',(-3.,10.,18.));
#21783=CARTESIAN_POINT('',(-3.,10.,18.));
#21784=CARTESIAN_POINT('',(-3.,10.,19.));
#21785=CARTESIAN_POINT('Origin',(22.5,0.,19.));
#21786=CARTESIAN_POINT('Origin',(22.5,0.,18.));
#21787=CARTESIAN_POINT('',(0.,0.,0.));
#21788=CARTESIAN_POINT('Origin',(1.5,-4.,16.9));
#21789=CARTESIAN_POINT('',(1.29,-4.,17.));
#21790=CARTESIAN_POINT('Origin',(1.5,-4.,17.));
#21791=CARTESIAN_POINT('',(1.29,-4.,18.));
#21792=CARTESIAN_POINT('',(1.29,-4.,16.9));
#21793=CARTESIAN_POINT('Origin',(1.5,-4.,18.));
#21794=CARTESIAN_POINT('Origin',(-1.5,4.,16.9));
#21795=CARTESIAN_POINT('',(-1.71,4.,17.));
#21796=CARTESIAN_POINT('Origin',(-1.5,4.,17.));
#21797=CARTESIAN_POINT('',(-1.71,4.,18.));
#21798=CARTESIAN_POINT('',(-1.71,4.,16.9));
#21799=CARTESIAN_POINT('Origin',(-1.5,4.,18.));
#21800=CARTESIAN_POINT('Origin',(-1.5,-4.,16.9));
#21801=CARTESIAN_POINT('',(-1.71,-4.,17.));
#21802=CARTESIAN_POINT('Origin',(-1.5,-4.,17.));
#21803=CARTESIAN_POINT('',(-1.71,-4.,18.));
#21804=CARTESIAN_POINT('',(-1.71,-4.,16.9));
#21805=CARTESIAN_POINT('Origin',(-1.5,-4.,18.));
#21806=CARTESIAN_POINT('Origin',(1.5,4.,16.9));
#21807=CARTESIAN_POINT('',(1.29,4.,17.));
#21808=CARTESIAN_POINT('Origin',(1.5,4.,17.));
#21809=CARTESIAN_POINT('',(1.29,4.,18.));
#21810=CARTESIAN_POINT('',(1.29,4.,16.9));
#21811=CARTESIAN_POINT('Origin',(1.5,4.,18.));
#21812=CARTESIAN_POINT('Origin',(0.,0.,17.));
#21813=CARTESIAN_POINT('',(-2.,5.,17.));
#21814=CARTESIAN_POINT('',(-2.,-5.,17.));
#21815=CARTESIAN_POINT('',(-2.,5.,17.));
#21816=CARTESIAN_POINT('',(2.,5.,17.));
#21817=CARTESIAN_POINT('',(2.,5.,17.));
#21818=CARTESIAN_POINT('',(2.,-5.,17.));
#21819=CARTESIAN_POINT('',(2.,-5.,17.));
#21820=CARTESIAN_POINT('',(-2.,-5.,17.));
#21821=CARTESIAN_POINT('',(-1.,4.,17.));
#21822=CARTESIAN_POINT('',(1.,4.,17.));
#21823=CARTESIAN_POINT('',(0.5,4.,17.));
#21824=CARTESIAN_POINT('',(-1.,-4.,17.));
#21825=CARTESIAN_POINT('',(-1.,2.,17.));
#21826=CARTESIAN_POINT('',(1.,-4.,17.));
#21827=CARTESIAN_POINT('',(-0.5,-4.,17.));
#21828=CARTESIAN_POINT('',(1.,-2.,17.));
#21829=CARTESIAN_POINT('Origin',(2.,5.,17.));
#21830=CARTESIAN_POINT('',(-2.,5.,18.));
#21831=CARTESIAN_POINT('',(-2.,5.,17.));
#21832=CARTESIAN_POINT('',(2.,5.,18.));
#21833=CARTESIAN_POINT('',(2.,5.,18.));
#21834=CARTESIAN_POINT('',(2.,5.,17.));
#21835=CARTESIAN_POINT('Origin',(2.,-5.,17.));
#21836=CARTESIAN_POINT('',(2.,-5.,18.));
#21837=CARTESIAN_POINT('',(2.,-5.,18.));
#21838=CARTESIAN_POINT('',(2.,-5.,17.));
#21839=CARTESIAN_POINT('Origin',(-2.,-5.,17.));
#21840=CARTESIAN_POINT('',(-2.,-5.,18.));
#21841=CARTESIAN_POINT('',(-2.,-5.,18.));
#21842=CARTESIAN_POINT('',(-2.,-5.,17.));
#21843=CARTESIAN_POINT('Origin',(-2.,5.,17.));
#21844=CARTESIAN_POINT('',(-2.,5.,18.));
#21845=CARTESIAN_POINT('Origin',(-1.,-4.,11.));
#21846=CARTESIAN_POINT('',(-1.,-4.,11.));
#21847=CARTESIAN_POINT('',(-1.,-4.,11.));
#21848=CARTESIAN_POINT('',(1.,-4.,11.));
#21849=CARTESIAN_POINT('',(-1.,-4.,11.));
#21850=CARTESIAN_POINT('',(1.,-4.,11.));
#21851=CARTESIAN_POINT('',(-0.605,-4.,13.));
#21852=CARTESIAN_POINT('Origin',(0.,-4.,13.));
#21853=CARTESIAN_POINT('Origin',(-1.,4.,11.));
#21854=CARTESIAN_POINT('',(-1.,4.,11.));
#21855=CARTESIAN_POINT('',(-1.,4.,11.));
#21856=CARTESIAN_POINT('',(-1.,4.,11.));
#21857=CARTESIAN_POINT('',(-1.,3.,16.605));
#21858=CARTESIAN_POINT('Origin',(-1.,3.,16.));
#21859=CARTESIAN_POINT('',(-1.,-3.,16.605));
#21860=CARTESIAN_POINT('Origin',(-1.,-3.,16.));
#21861=CARTESIAN_POINT('Origin',(0.,-5.1,13.));
#21862=CARTESIAN_POINT('',(-0.605,4.,13.));
#21863=CARTESIAN_POINT('',(-0.605,-5.1,13.));
#21864=CARTESIAN_POINT('Origin',(0.,4.,13.));
#21865=CARTESIAN_POINT('Origin',(-1.1,-3.,16.));
#21866=CARTESIAN_POINT('',(1.,-3.,16.605));
#21867=CARTESIAN_POINT('',(-1.1,-3.,16.605));
#21868=CARTESIAN_POINT('Origin',(1.,-3.,16.));
#21869=CARTESIAN_POINT('Origin',(-1.1,3.,16.));
#21870=CARTESIAN_POINT('',(1.,3.,16.605));
#21871=CARTESIAN_POINT('',(-1.1,3.,16.605));
#21872=CARTESIAN_POINT('Origin',(1.,3.,16.));
#21873=CARTESIAN_POINT('Origin',(1.,4.,11.));
#21874=CARTESIAN_POINT('',(1.,4.,11.));
#21875=CARTESIAN_POINT('',(1.,4.,11.));
#21876=CARTESIAN_POINT('',(1.,4.,11.));
#21877=CARTESIAN_POINT('Origin',(1.,-4.,11.));
#21878=CARTESIAN_POINT('',(1.,-4.,11.));
#21879=CARTESIAN_POINT('Origin',(0.,0.,18.));
#21880=CARTESIAN_POINT('Origin',(0.,0.,11.));
#21881=CARTESIAN_POINT('',(0.,0.,0.));
#21882=CARTESIAN_POINT('Origin',(46.5,-4.,16.9));
#21883=CARTESIAN_POINT('',(46.29,-4.,17.));
#21884=CARTESIAN_POINT('Origin',(46.5,-4.,17.));
#21885=CARTESIAN_POINT('',(46.29,-4.,18.));
#21886=CARTESIAN_POINT('',(46.29,-4.,16.9));
#21887=CARTESIAN_POINT('Origin',(46.5,-4.,18.));
#21888=CARTESIAN_POINT('Origin',(43.5,4.,16.9));
#21889=CARTESIAN_POINT('',(43.29,4.,17.));
#21890=CARTESIAN_POINT('Origin',(43.5,4.,17.));
#21891=CARTESIAN_POINT('',(43.29,4.,18.));
#21892=CARTESIAN_POINT('',(43.29,4.,16.9));
#21893=CARTESIAN_POINT('Origin',(43.5,4.,18.));
#21894=CARTESIAN_POINT('Origin',(43.5,-4.,16.9));
#21895=CARTESIAN_POINT('',(43.29,-4.,17.));
#21896=CARTESIAN_POINT('Origin',(43.5,-4.,17.));
#21897=CARTESIAN_POINT('',(43.29,-4.,18.));
#21898=CARTESIAN_POINT('',(43.29,-4.,16.9));
#21899=CARTESIAN_POINT('Origin',(43.5,-4.,18.));
#21900=CARTESIAN_POINT('Origin',(46.5,4.,16.9));
#21901=CARTESIAN_POINT('',(46.29,4.,17.));
#21902=CARTESIAN_POINT('Origin',(46.5,4.,17.));
#21903=CARTESIAN_POINT('',(46.29,4.,18.));
#21904=CARTESIAN_POINT('',(46.29,4.,16.9));
#21905=CARTESIAN_POINT('Origin',(46.5,4.,18.));
#21906=CARTESIAN_POINT('Origin',(45.,0.,17.));
#21907=CARTESIAN_POINT('',(44.,-5.,17.));
#21908=CARTESIAN_POINT('',(44.,5.,17.));
#21909=CARTESIAN_POINT('',(44.,2.5,17.));
#21910=CARTESIAN_POINT('',(43.,-5.,17.));
#21911=CARTESIAN_POINT('',(43.,-5.,17.));
#21912=CARTESIAN_POINT('',(43.,5.,17.));
#21913=CARTESIAN_POINT('',(43.,5.,17.));
#21914=CARTESIAN_POINT('',(47.,5.,17.));
#21915=CARTESIAN_POINT('Origin',(47.,-5.,17.));
#21916=CARTESIAN_POINT('',(47.,-5.,17.));
#21917=CARTESIAN_POINT('',(47.,5.,17.));
#21918=CARTESIAN_POINT('',(47.,-5.,17.));
#21919=CARTESIAN_POINT('',(47.,5.,18.));
#21920=CARTESIAN_POINT('',(47.,5.,17.));
#21921=CARTESIAN_POINT('',(47.,-5.,18.));
#21922=CARTESIAN_POINT('',(47.,-5.,18.));
#21923=CARTESIAN_POINT('',(47.,-5.,17.));
#21924=CARTESIAN_POINT('Origin',(43.,5.,17.));
#21925=CARTESIAN_POINT('',(43.,-5.,18.));
#21926=CARTESIAN_POINT('',(43.,-5.,17.));
#21927=CARTESIAN_POINT('',(43.,5.,18.));
#21928=CARTESIAN_POINT('',(43.,5.,18.));
#21929=CARTESIAN_POINT('',(43.,5.,17.));
#21930=CARTESIAN_POINT('Origin',(45.,0.,17.));
#21931=CARTESIAN_POINT('',(46.,5.,17.));
#21932=CARTESIAN_POINT('',(46.,-5.,17.));
#21933=CARTESIAN_POINT('',(46.,-2.5,17.));
#21934=CARTESIAN_POINT('',(47.,5.,17.));
#21935=CARTESIAN_POINT('',(43.,-5.,17.));
#21936=CARTESIAN_POINT('Origin',(46.,-5.,14.));
#21937=CARTESIAN_POINT('',(46.,-5.,14.));
#21938=CARTESIAN_POINT('',(46.,-5.,14.));
#21939=CARTESIAN_POINT('',(46.,5.,14.));
#21940=CARTESIAN_POINT('',(46.,-5.,14.));
#21941=CARTESIAN_POINT('',(46.,5.,14.));
#21942=CARTESIAN_POINT('',(46.,3.,16.605));
#21943=CARTESIAN_POINT('Origin',(46.,3.,16.));
#21944=CARTESIAN_POINT('',(46.,-3.,16.605));
#21945=CARTESIAN_POINT('Origin',(46.,-3.,16.));
#21946=CARTESIAN_POINT('Origin',(44.,-5.,14.));
#21947=CARTESIAN_POINT('',(44.,-5.,14.));
#21948=CARTESIAN_POINT('',(44.,-5.,14.));
#21949=CARTESIAN_POINT('',(44.,-5.,14.));
#21950=CARTESIAN_POINT('',(43.,-5.,18.));
#21951=CARTESIAN_POINT('Origin',(43.9,-3.,16.));
#21952=CARTESIAN_POINT('',(44.,-3.,16.605));
#21953=CARTESIAN_POINT('Origin',(44.,-3.,16.));
#21954=CARTESIAN_POINT('',(43.9,-3.,16.605));
#21955=CARTESIAN_POINT('Origin',(43.9,3.,16.));
#21956=CARTESIAN_POINT('',(44.,3.,16.605));
#21957=CARTESIAN_POINT('Origin',(44.,3.,16.));
#21958=CARTESIAN_POINT('',(43.9,3.,16.605));
#21959=CARTESIAN_POINT('Origin',(46.,5.,14.));
#21960=CARTESIAN_POINT('',(44.,5.,14.));
#21961=CARTESIAN_POINT('',(46.,5.,14.));
#21962=CARTESIAN_POINT('',(44.,5.,14.));
#21963=CARTESIAN_POINT('',(47.,5.,18.));
#21964=CARTESIAN_POINT('Origin',(44.,5.,14.));
#21965=CARTESIAN_POINT('',(44.,5.,14.));
#21966=CARTESIAN_POINT('Origin',(45.,0.,18.));
#21967=CARTESIAN_POINT('Origin',(45.,0.,14.));
#21968=CARTESIAN_POINT('',(0.,0.,0.));
#21969=CARTESIAN_POINT('Origin',(-1.,-3.,16.));
#21970=CARTESIAN_POINT('',(47.,-3.,16.6));
#21971=CARTESIAN_POINT('Origin',(47.,-3.,16.));
#21972=CARTESIAN_POINT('',(-1.,-3.,16.6));
#21973=CARTESIAN_POINT('',(-1.,-3.,16.6));
#21974=CARTESIAN_POINT('Origin',(-1.,-3.,16.));
#21975=CARTESIAN_POINT('Origin',(47.,-3.,16.));
#21976=CARTESIAN_POINT('Origin',(-1.,-3.,16.));
#21977=CARTESIAN_POINT('',(0.,0.,0.));
#21978=CARTESIAN_POINT('Origin',(-1.,3.,16.));
#21979=CARTESIAN_POINT('',(47.,3.,16.6));
#21980=CARTESIAN_POINT('Origin',(47.,3.,16.));
#21981=CARTESIAN_POINT('',(-1.,3.,16.6));
#21982=CARTESIAN_POINT('',(-1.,3.,16.6));
#21983=CARTESIAN_POINT('Origin',(-1.,3.,16.));
#21984=CARTESIAN_POINT('Origin',(47.,3.,16.));
#21985=CARTESIAN_POINT('Origin',(-1.,3.,16.));
#21986=CARTESIAN_POINT('',(0.,0.,0.));
#21987=CARTESIAN_POINT('Origin',(0.,6.9,13.));
#21988=CARTESIAN_POINT('',(-0.165,6.9,13.));
#21989=CARTESIAN_POINT('Origin',(0.,6.9,13.));
#21990=CARTESIAN_POINT('',(-0.165,8.5,13.));
#21991=CARTESIAN_POINT('',(-0.165,6.9,13.));
#21992=CARTESIAN_POINT('Origin',(0.,8.5,13.));
#21993=CARTESIAN_POINT('Origin',(0.,6.9,13.));
#21994=CARTESIAN_POINT('Origin',(0.,-6.1,13.));
#21995=CARTESIAN_POINT('',(-0.165,-6.,13.));
#21996=CARTESIAN_POINT('Origin',(0.,-6.,13.));
#21997=CARTESIAN_POINT('',(-0.165,-4.4,13.));
#21998=CARTESIAN_POINT('',(-0.165,-6.1,13.));
#21999=CARTESIAN_POINT('Origin',(0.,-4.4,13.));
#22000=CARTESIAN_POINT('Origin',(0.,-4.4,13.));
#22001=CARTESIAN_POINT('Origin',(0.,-6.,13.));
#22002=CARTESIAN_POINT('',(-0.6,8.5,13.));
#22003=CARTESIAN_POINT('Origin',(0.,8.5,13.));
#22004=CARTESIAN_POINT('',(-0.6,-6.,13.));
#22005=CARTESIAN_POINT('',(-0.6,-6.,13.));
#22006=CARTESIAN_POINT('Origin',(0.,-6.,13.));
#22007=CARTESIAN_POINT('Origin',(0.,8.5,13.));
#22008=CARTESIAN_POINT('Origin',(0.,-6.,13.));
#22009=CARTESIAN_POINT('',(0.,0.,0.));
#22010=CARTESIAN_POINT('Origin',(0.,-6.2,13.));
#22011=CARTESIAN_POINT('',(-0.225,-6.,13.));
#22012=CARTESIAN_POINT('Origin',(0.,-6.,13.));
#22013=CARTESIAN_POINT('',(-0.225,-6.2,13.));
#22014=CARTESIAN_POINT('',(-0.225,-6.2,13.));
#22015=CARTESIAN_POINT('Origin',(0.,-6.2,13.));
#22016=CARTESIAN_POINT('Origin',(0.,-6.2,13.));
#22017=CARTESIAN_POINT('',(-1.,-6.,13.));
#22018=CARTESIAN_POINT('Origin',(0.,-6.,13.));
#22019=CARTESIAN_POINT('',(-1.,-6.2,13.));
#22020=CARTESIAN_POINT('',(-1.,-6.2,13.));
#22021=CARTESIAN_POINT('Origin',(0.,-6.2,13.));
#22022=CARTESIAN_POINT('Origin',(0.,-6.,13.));
#22023=CARTESIAN_POINT('Origin',(0.,-6.2,13.));
#22024=CARTESIAN_POINT('',(0.,0.,0.));
#22025=CARTESIAN_POINT('Origin',(0.,8.5,13.));
#22026=CARTESIAN_POINT('',(-0.225,8.7,13.));
#22027=CARTESIAN_POINT('Origin',(0.,8.7,13.));
#22028=CARTESIAN_POINT('',(-0.225,8.5,13.));
#22029=CARTESIAN_POINT('',(-0.225,8.5,13.));
#22030=CARTESIAN_POINT('Origin',(0.,8.5,13.));
#22031=CARTESIAN_POINT('Origin',(0.,8.5,13.));
#22032=CARTESIAN_POINT('',(-1.,8.7,13.));
#22033=CARTESIAN_POINT('Origin',(0.,8.7,13.));
#22034=CARTESIAN_POINT('',(-1.,8.5,13.));
#22035=CARTESIAN_POINT('',(-1.,8.5,13.));
#22036=CARTESIAN_POINT('Origin',(0.,8.5,13.));
#22037=CARTESIAN_POINT('Origin',(0.,8.7,13.));
#22038=CARTESIAN_POINT('Origin',(0.,8.5,13.));
#22039=CARTESIAN_POINT('',(0.,0.,0.));
#22040=CARTESIAN_POINT('Origin',(0.,-6.,13.));
#22041=CARTESIAN_POINT('',(-0.605,-5.5,13.));
#22042=CARTESIAN_POINT('Origin',(0.,-5.5,13.));
#22043=CARTESIAN_POINT('',(-0.605,-6.,13.));
#22044=CARTESIAN_POINT('',(-0.605,-6.,13.));
#22045=CARTESIAN_POINT('Origin',(0.,-6.,13.));
#22046=CARTESIAN_POINT('Origin',(0.,-6.,13.));
#22047=CARTESIAN_POINT('',(-0.8,-5.5,13.));
#22048=CARTESIAN_POINT('Origin',(0.,-5.5,13.));
#22049=CARTESIAN_POINT('',(-0.8,-6.,13.));
#22050=CARTESIAN_POINT('',(-0.8,-6.,13.));
#22051=CARTESIAN_POINT('Origin',(0.,-6.,13.));
#22052=CARTESIAN_POINT('Origin',(0.,-5.5,13.));
#22053=CARTESIAN_POINT('Origin',(0.,-6.,13.));
#22054=CARTESIAN_POINT('',(0.,0.,0.));
#22055=CARTESIAN_POINT('Origin',(0.,-4.5,13.));
#22056=CARTESIAN_POINT('',(-0.605,-4.,13.));
#22057=CARTESIAN_POINT('Origin',(0.,-4.,13.));
#22058=CARTESIAN_POINT('',(-0.605,-4.5,13.));
#22059=CARTESIAN_POINT('',(-0.605,-4.5,13.));
#22060=CARTESIAN_POINT('Origin',(0.,-4.5,13.));
#22061=CARTESIAN_POINT('Origin',(0.,-4.5,13.));
#22062=CARTESIAN_POINT('',(-0.8,-4.,13.));
#22063=CARTESIAN_POINT('Origin',(0.,-4.,13.));
#22064=CARTESIAN_POINT('',(-0.8,-4.5,13.));
#22065=CARTESIAN_POINT('',(-0.8,-4.5,13.));
#22066=CARTESIAN_POINT('Origin',(0.,-4.5,13.));
#22067=CARTESIAN_POINT('Origin',(0.,-4.,13.));
#22068=CARTESIAN_POINT('Origin',(0.,-4.5,13.));
#22069=CARTESIAN_POINT('',(0.,0.,0.));
#22070=CARTESIAN_POINT('Origin',(0.,4.,13.));
#22071=CARTESIAN_POINT('',(-0.605,7.,13.));
#22072=CARTESIAN_POINT('Origin',(0.,7.,13.));
#22073=CARTESIAN_POINT('',(-0.605,4.,13.));
#22074=CARTESIAN_POINT('',(-0.605,4.,13.));
#22075=CARTESIAN_POINT('Origin',(0.,4.,13.));
#22076=CARTESIAN_POINT('Origin',(0.,4.,13.));
#22077=CARTESIAN_POINT('',(-0.8,7.,13.));
#22078=CARTESIAN_POINT('Origin',(0.,7.,13.));
#22079=CARTESIAN_POINT('',(-0.8,4.,13.));
#22080=CARTESIAN_POINT('',(-0.8,4.,13.));
#22081=CARTESIAN_POINT('Origin',(0.,4.,13.));
#22082=CARTESIAN_POINT('Origin',(0.,7.,13.));
#22083=CARTESIAN_POINT('Origin',(0.,4.,13.));
#22084=CARTESIAN_POINT('',(0.,0.,0.));
#22085=CARTESIAN_POINT('Origin',(0.,8.,13.));
#22086=CARTESIAN_POINT('',(-0.605,8.5,13.));
#22087=CARTESIAN_POINT('Origin',(0.,8.5,13.));
#22088=CARTESIAN_POINT('',(-0.605,8.,13.));
#22089=CARTESIAN_POINT('',(-0.605,8.,13.));
#22090=CARTESIAN_POINT('Origin',(0.,8.,13.));
#22091=CARTESIAN_POINT('Origin',(0.,8.,13.));
#22092=CARTESIAN_POINT('',(-0.8,8.5,13.));
#22093=CARTESIAN_POINT('Origin',(0.,8.5,13.));
#22094=CARTESIAN_POINT('',(-0.8,8.,13.));
#22095=CARTESIAN_POINT('',(-0.8,8.,13.));
#22096=CARTESIAN_POINT('Origin',(0.,8.,13.));
#22097=CARTESIAN_POINT('Origin',(0.,8.5,13.));
#22098=CARTESIAN_POINT('Origin',(0.,8.,13.));
#22099=CARTESIAN_POINT('',(0.,0.,0.));
#22100=CARTESIAN_POINT('Origin',(0.375,0.5,0.));
#22101=CARTESIAN_POINT('',(-0.375,0.5,-4.59242549680257E-17));
#22102=CARTESIAN_POINT('Origin',(0.,0.5,0.));
#22103=CARTESIAN_POINT('Origin',(0.,0.475,0.));
#22104=CARTESIAN_POINT('',(-0.425,0.45,-5.20474889637625E-17));
#22105=CARTESIAN_POINT('Origin',(0.,0.45,0.));
#22106=CARTESIAN_POINT('',(-0.4,0.475,-4.89858719658941E-17));
#22107=CARTESIAN_POINT('Origin',(0.,0.24,0.));
#22108=CARTESIAN_POINT('',(-0.425,0.0299999999999998,-5.20474889637625E-17));
#22109=CARTESIAN_POINT('Origin',(0.,0.0299999999999998,0.));
#22110=CARTESIAN_POINT('',(-0.425,0.24,-5.20474889637625E-17));
#22111=CARTESIAN_POINT('Origin',(0.,0.0150000000000001,0.));
#22112=CARTESIAN_POINT('',(-0.395,4.85722573273506E-17,-4.83735485663204E-17));
#22113=CARTESIAN_POINT('Origin',(0.,0.,0.));
#22114=CARTESIAN_POINT('',(-0.41,0.0150000000000001,-5.02105187650415E-17));
#22115=CARTESIAN_POINT('Origin',(0.27,0.,0.));
#22116=CARTESIAN_POINT('',(-0.27,0.,-3.30654635769785E-17));
#22117=CARTESIAN_POINT('Origin',(0.,0.,0.));
#22118=CARTESIAN_POINT('Origin',(0.,-0.02,0.));
#22119=CARTESIAN_POINT('',(-0.24505,-0.0498999999999999,3.00099698131059E-17));
#22120=CARTESIAN_POINT('Origin',(0.,-0.0498999999999999,0.));
#22121=CARTESIAN_POINT('',(-0.26,-0.02,-3.18408167778312E-17));
#22122=CARTESIAN_POINT('Origin',(0.,-0.995,0.));
#22123=CARTESIAN_POINT('',(-0.24505,-1.95495,3.00099698131059E-17));
#22124=CARTESIAN_POINT('Origin',(0.,-1.95495,0.));
#22125=CARTESIAN_POINT('',(-0.24505,-0.995,-3.00099698131059E-17));
#22126=CARTESIAN_POINT('Origin',(0.,-1.975,0.));
#22127=CARTESIAN_POINT('',(-0.2,-2.,-2.44929359829471E-17));
#22128=CARTESIAN_POINT('Origin',(0.,-2.,0.));
#22129=CARTESIAN_POINT('',(-0.225,-1.975,-2.75545529808154E-17));
#22130=CARTESIAN_POINT('Origin',(0.,-2.,0.));
#22131=CARTESIAN_POINT('Origin',(0.115470053837925,-0.5,-0.2));
#22132=CARTESIAN_POINT('',(0.23094010767585,-0.5,0.));
#22133=CARTESIAN_POINT('',(0.115470053837925,-0.5,-0.2));
#22134=CARTESIAN_POINT('',(0.23094010767585,-0.5,0.));
#22135=CARTESIAN_POINT('',(0.115470053837925,-0.8,-0.2));
#22136=CARTESIAN_POINT('',(0.115470053837925,-0.5,-0.2));
#22137=CARTESIAN_POINT('',(0.23094010767585,-0.8,0.));
#22138=CARTESIAN_POINT('',(0.23094010767585,-0.8,0.));
#22139=CARTESIAN_POINT('',(0.23094010767585,-0.5,0.));
#22140=CARTESIAN_POINT('Origin',(-0.115470053837925,-0.5,-0.2));
#22141=CARTESIAN_POINT('',(-0.115470053837925,-0.5,-0.2));
#22142=CARTESIAN_POINT('',(0.115470053837925,-0.5,-0.2));
#22143=CARTESIAN_POINT('',(-0.115470053837925,-0.8,-0.2));
#22144=CARTESIAN_POINT('',(-0.115470053837925,-0.5,-0.2));
#22145=CARTESIAN_POINT('',(0.115470053837925,-0.8,-0.2));
#22146=CARTESIAN_POINT('Origin',(-0.23094010767585,-0.5,-2.77555756156289E-17));
#22147=CARTESIAN_POINT('',(-0.23094010767585,-0.5,-2.82820063659975E-17));
#22148=CARTESIAN_POINT('',(-0.115470053837925,-0.5,-0.2));
#22149=CARTESIAN_POINT('',(-0.23094010767585,-0.8,-2.77555756156289E-17));
#22150=CARTESIAN_POINT('',(-0.23094010767585,-0.5,-2.82820063659975E-17));
#22151=CARTESIAN_POINT('',(-0.115470053837925,-0.8,-0.2));
#22152=CARTESIAN_POINT('Origin',(-0.115470053837925,-0.5,0.2));
#22153=CARTESIAN_POINT('',(-0.115470053837925,-0.5,0.2));
#22154=CARTESIAN_POINT('',(-0.23094010767585,-0.5,-2.82820063659975E-17));
#22155=CARTESIAN_POINT('',(-0.115470053837925,-0.8,0.2));
#22156=CARTESIAN_POINT('',(-0.115470053837925,-0.5,0.2));
#22157=CARTESIAN_POINT('',(-0.23094010767585,-0.8,-2.82820063659975E-17));
#22158=CARTESIAN_POINT('Origin',(0.115470053837925,-0.5,0.2));
#22159=CARTESIAN_POINT('',(0.115470053837925,-0.5,0.2));
#22160=CARTESIAN_POINT('',(-0.115470053837925,-0.5,0.2));
#22161=CARTESIAN_POINT('',(0.115470053837925,-0.8,0.2));
#22162=CARTESIAN_POINT('',(0.115470053837925,-0.5,0.2));
#22163=CARTESIAN_POINT('',(-0.115470053837925,-0.8,0.2));
#22164=CARTESIAN_POINT('Origin',(0.23094010767585,-0.5,0.));
#22165=CARTESIAN_POINT('',(0.115470053837925,-0.5,0.2));
#22166=CARTESIAN_POINT('',(0.115470053837925,-0.8,0.2));
#22167=CARTESIAN_POINT('Origin',(0.,-0.5,0.));
#22168=CARTESIAN_POINT('Origin',(0.,-0.8,0.));
#22169=CARTESIAN_POINT('',(0.,0.,0.));
#22170=CARTESIAN_POINT('',(0.,0.,0.));
#22171=CARTESIAN_POINT('Origin',(36.92983346,0.,6.));
#22172=CARTESIAN_POINT('',(37.0298334620742,-6.12323399573677E-17,6.5));
#22173=CARTESIAN_POINT('Origin',(37.0298334620742,0.,6.));
#22174=CARTESIAN_POINT('',(40.4298334620742,6.12323399573677E-17,6.5));
#22175=CARTESIAN_POINT('',(36.92983346,-6.12323399573677E-17,6.5));
#22176=CARTESIAN_POINT('Origin',(40.4298334620742,0.,6.));
#22177=CARTESIAN_POINT('Origin',(36.92983346,-3.,6.));
#22178=CARTESIAN_POINT('',(37.0298334620742,-3.,7.05));
#22179=CARTESIAN_POINT('Origin',(37.0298334620742,-3.,6.));
#22180=CARTESIAN_POINT('',(40.4298334620742,-3.,7.05));
#22181=CARTESIAN_POINT('',(36.92983346,-3.,7.05));
#22182=CARTESIAN_POINT('Origin',(40.4298334620742,-3.,6.));
#22183=CARTESIAN_POINT('Origin',(36.92983346,3.,6.));
#22184=CARTESIAN_POINT('',(37.0298334620742,3.,7.05));
#22185=CARTESIAN_POINT('Origin',(37.0298334620742,3.,6.));
#22186=CARTESIAN_POINT('',(40.4298334620742,3.,7.05));
#22187=CARTESIAN_POINT('',(36.92983346,3.,7.05));
#22188=CARTESIAN_POINT('Origin',(40.4298334620742,3.,6.));
#22189=CARTESIAN_POINT('Origin',(40.4298334620742,4.7,4.3));
#22190=CARTESIAN_POINT('',(40.4298334620742,4.7,4.3));
#22191=CARTESIAN_POINT('',(37.0298334620742,4.7,4.3));
#22192=CARTESIAN_POINT('',(40.4298334620742,4.7,4.3));
#22193=CARTESIAN_POINT('',(37.0298334620742,4.7,7.7));
#22194=CARTESIAN_POINT('',(37.0298334620742,4.7,4.3));
#22195=CARTESIAN_POINT('',(40.4298334620742,4.7,7.7));
#22196=CARTESIAN_POINT('',(40.4298334620742,4.7,7.7));
#22197=CARTESIAN_POINT('',(40.4298334620742,4.7,4.3));
#22198=CARTESIAN_POINT('Origin',(40.4298334620742,-4.3,4.3));
#22199=CARTESIAN_POINT('',(40.4298334620742,-4.3,4.3));
#22200=CARTESIAN_POINT('',(40.4298334620742,-4.3,4.3));
#22201=CARTESIAN_POINT('',(40.4298334620742,-4.3,7.7));
#22202=CARTESIAN_POINT('',(40.4298334620742,-4.3,7.7));
#22203=CARTESIAN_POINT('',(40.4298334620742,-4.3,4.3));
#22204=CARTESIAN_POINT('Origin',(37.0298334620742,-4.3,4.3));
#22205=CARTESIAN_POINT('',(37.0298334620742,-4.3,4.3));
#22206=CARTESIAN_POINT('',(37.0298334620742,-4.3,4.3));
#22207=CARTESIAN_POINT('',(37.0298334620742,-4.3,7.7));
#22208=CARTESIAN_POINT('',(37.0298334620742,-4.3,7.7));
#22209=CARTESIAN_POINT('',(37.0298334620742,-4.3,4.3));
#22210=CARTESIAN_POINT('Origin',(37.0298334620742,4.7,4.3));
#22211=CARTESIAN_POINT('',(37.0298334620742,4.7,4.3));
#22212=CARTESIAN_POINT('',(37.0298334620742,4.7,7.7));
#22213=CARTESIAN_POINT('Origin',(38.7298334620742,0.2,7.7));
#22214=CARTESIAN_POINT('Origin',(38.7298334620742,0.2,4.3));
#22215=CARTESIAN_POINT('',(0.,0.,0.));
#22216=CARTESIAN_POINT('Origin',(37.02983346,3.,6.));
#22217=CARTESIAN_POINT('',(37.22983346,3.,7.04));
#22218=CARTESIAN_POINT('Origin',(37.22983346,3.,6.));
#22219=CARTESIAN_POINT('',(37.02983346,3.,7.04));
#22220=CARTESIAN_POINT('',(37.02983346,3.,7.04));
#22221=CARTESIAN_POINT('Origin',(37.02983346,3.,6.));
#22222=CARTESIAN_POINT('Origin',(37.22983346,3.,6.));
#22223=CARTESIAN_POINT('',(37.22983346,3.,6.8));
#22224=CARTESIAN_POINT('Origin',(37.22983346,3.,6.));
#22225=CARTESIAN_POINT('Origin',(37.02983346,-3.,6.));
#22226=CARTESIAN_POINT('',(37.22983346,-3.,7.04));
#22227=CARTESIAN_POINT('Origin',(37.22983346,-3.,6.));
#22228=CARTESIAN_POINT('',(37.02983346,-3.,7.04));
#22229=CARTESIAN_POINT('',(37.02983346,-3.,7.04));
#22230=CARTESIAN_POINT('Origin',(37.02983346,-3.,6.));
#22231=CARTESIAN_POINT('Origin',(37.22983346,-3.,6.));
#22232=CARTESIAN_POINT('',(37.22983346,-3.,6.8));
#22233=CARTESIAN_POINT('Origin',(37.22983346,-3.,6.));
#22234=CARTESIAN_POINT('Origin',(36.72983346,0.,6.));
#22235=CARTESIAN_POINT('',(36.82983346,-7.9602041944578E-17,6.65));
#22236=CARTESIAN_POINT('Origin',(36.82983346,0.,6.));
#22237=CARTESIAN_POINT('',(37.02983346,7.9602041944578E-17,6.65));
#22238=CARTESIAN_POINT('',(36.72983346,-7.9602041944578E-17,6.65));
#22239=CARTESIAN_POINT('Origin',(37.02983346,0.,6.));
#22240=CARTESIAN_POINT('Origin',(36.72983346,-3.,6.));
#22241=CARTESIAN_POINT('',(36.82983346,-3.,6.8));
#22242=CARTESIAN_POINT('Origin',(36.82983346,-3.,6.));
#22243=CARTESIAN_POINT('',(36.72983346,-3.,6.8));
#22244=CARTESIAN_POINT('Origin',(36.72983346,3.,6.));
#22245=CARTESIAN_POINT('',(36.82983346,3.,6.8));
#22246=CARTESIAN_POINT('Origin',(36.82983346,3.,6.));
#22247=CARTESIAN_POINT('',(36.72983346,3.,6.8));
#22248=CARTESIAN_POINT('Origin',(36.82983346,4.7,7.7));
#22249=CARTESIAN_POINT('',(36.82983346,4.7,7.7));
#22250=CARTESIAN_POINT('',(36.82983346,-4.3,7.7));
#22251=CARTESIAN_POINT('',(36.82983346,4.7,7.7));
#22252=CARTESIAN_POINT('',(37.02983346,-4.3,7.7));
#22253=CARTESIAN_POINT('',(36.82983346,-4.3,7.7));
#22254=CARTESIAN_POINT('',(37.02983346,4.7,7.7));
#22255=CARTESIAN_POINT('',(37.02983346,4.7,7.7));
#22256=CARTESIAN_POINT('',(36.82983346,4.7,7.7));
#22257=CARTESIAN_POINT('Origin',(36.82983346,4.7,4.3));
#22258=CARTESIAN_POINT('',(36.82983346,4.7,4.3));
#22259=CARTESIAN_POINT('',(36.82983346,4.7,4.3));
#22260=CARTESIAN_POINT('',(37.02983346,4.7,4.3));
#22261=CARTESIAN_POINT('',(37.02983346,4.7,4.3));
#22262=CARTESIAN_POINT('',(36.82983346,4.7,4.3));
#22263=CARTESIAN_POINT('Origin',(36.82983346,-4.3,4.3));
#22264=CARTESIAN_POINT('',(36.82983346,-4.3,4.3));
#22265=CARTESIAN_POINT('',(36.82983346,-4.3,4.3));
#22266=CARTESIAN_POINT('',(37.02983346,-4.3,4.3));
#22267=CARTESIAN_POINT('',(37.02983346,-4.3,4.3));
#22268=CARTESIAN_POINT('',(36.82983346,-4.3,4.3));
#22269=CARTESIAN_POINT('Origin',(36.82983346,-4.3,7.7));
#22270=CARTESIAN_POINT('',(36.82983346,-4.3,7.7));
#22271=CARTESIAN_POINT('',(37.02983346,-4.3,7.7));
#22272=CARTESIAN_POINT('Origin',(37.02983346,0.2,6.));
#22273=CARTESIAN_POINT('Origin',(36.82983346,0.2,6.));
#22274=CARTESIAN_POINT('',(0.,0.,0.));
#22275=CARTESIAN_POINT('Origin',(40.22983346,3.,6.));
#22276=CARTESIAN_POINT('',(40.42983346,3.,7.04));
#22277=CARTESIAN_POINT('Origin',(40.42983346,3.,6.));
#22278=CARTESIAN_POINT('',(40.22983346,3.,7.04));
#22279=CARTESIAN_POINT('',(40.22983346,3.,7.04));
#22280=CARTESIAN_POINT('Origin',(40.22983346,3.,6.));
#22281=CARTESIAN_POINT('Origin',(40.22983346,3.,6.));
#22282=CARTESIAN_POINT('',(40.22983346,3.,6.8));
#22283=CARTESIAN_POINT('Origin',(40.22983346,3.,6.));
#22284=CARTESIAN_POINT('Origin',(40.22983346,-3.,6.));
#22285=CARTESIAN_POINT('',(40.42983346,-3.,7.04));
#22286=CARTESIAN_POINT('Origin',(40.42983346,-3.,6.));
#22287=CARTESIAN_POINT('',(40.22983346,-3.,7.04));
#22288=CARTESIAN_POINT('',(40.22983346,-3.,7.04));
#22289=CARTESIAN_POINT('Origin',(40.22983346,-3.,6.));
#22290=CARTESIAN_POINT('Origin',(40.22983346,-3.,6.));
#22291=CARTESIAN_POINT('',(40.22983346,-3.,6.8));
#22292=CARTESIAN_POINT('Origin',(40.22983346,-3.,6.));
#22293=CARTESIAN_POINT('Origin',(40.32983346,0.,6.));
#22294=CARTESIAN_POINT('',(40.42983346,-7.9602041944578E-17,6.65));
#22295=CARTESIAN_POINT('Origin',(40.42983346,0.,6.));
#22296=CARTESIAN_POINT('',(40.62983346,7.9602041944578E-17,6.65));
#22297=CARTESIAN_POINT('',(40.32983346,-7.9602041944578E-17,6.65));
#22298=CARTESIAN_POINT('Origin',(40.62983346,0.,6.));
#22299=CARTESIAN_POINT('Origin',(40.32983346,-3.,6.));
#22300=CARTESIAN_POINT('',(40.62983346,-3.,6.8));
#22301=CARTESIAN_POINT('',(40.32983346,-3.,6.8));
#22302=CARTESIAN_POINT('Origin',(40.62983346,-3.,6.));
#22303=CARTESIAN_POINT('Origin',(40.32983346,3.,6.));
#22304=CARTESIAN_POINT('',(40.62983346,3.,6.8));
#22305=CARTESIAN_POINT('',(40.32983346,3.,6.8));
#22306=CARTESIAN_POINT('Origin',(40.62983346,3.,6.));
#22307=CARTESIAN_POINT('Origin',(40.42983346,4.7,7.7));
#22308=CARTESIAN_POINT('',(40.42983346,4.7,7.7));
#22309=CARTESIAN_POINT('',(40.42983346,-4.3,7.7));
#22310=CARTESIAN_POINT('',(40.42983346,4.7,7.7));
#22311=CARTESIAN_POINT('',(40.62983346,-4.3,7.7));
#22312=CARTESIAN_POINT('',(40.42983346,-4.3,7.7));
#22313=CARTESIAN_POINT('',(40.62983346,4.7,7.7));
#22314=CARTESIAN_POINT('',(40.62983346,4.7,7.7));
#22315=CARTESIAN_POINT('',(40.42983346,4.7,7.7));
#22316=CARTESIAN_POINT('Origin',(40.42983346,4.7,4.3));
#22317=CARTESIAN_POINT('',(40.42983346,4.7,4.3));
#22318=CARTESIAN_POINT('',(40.42983346,4.7,4.3));
#22319=CARTESIAN_POINT('',(40.62983346,4.7,4.3));
#22320=CARTESIAN_POINT('',(40.62983346,4.7,4.3));
#22321=CARTESIAN_POINT('',(40.42983346,4.7,4.3));
#22322=CARTESIAN_POINT('Origin',(40.42983346,-4.3,4.3));
#22323=CARTESIAN_POINT('',(40.42983346,-4.3,4.3));
#22324=CARTESIAN_POINT('',(40.42983346,-4.3,4.3));
#22325=CARTESIAN_POINT('',(40.62983346,-4.3,4.3));
#22326=CARTESIAN_POINT('',(40.62983346,-4.3,4.3));
#22327=CARTESIAN_POINT('',(40.42983346,-4.3,4.3));
#22328=CARTESIAN_POINT('Origin',(40.42983346,-4.3,7.7));
#22329=CARTESIAN_POINT('',(40.42983346,-4.3,7.7));
#22330=CARTESIAN_POINT('',(40.62983346,-4.3,7.7));
#22331=CARTESIAN_POINT('Origin',(40.62983346,0.2,6.));
#22332=CARTESIAN_POINT('Origin',(40.42983346,0.2,6.));
#22333=CARTESIAN_POINT('',(0.,0.,0.));
#22334=CARTESIAN_POINT('Origin',(39.31983346,0.,3.));
#22335=CARTESIAN_POINT('',(39.31983346,-0.0964364949201869,2.86611571246965));
#22336=CARTESIAN_POINT('',(39.31983346,0.0964364949201869,2.86611571246965));
#22337=CARTESIAN_POINT('',(39.31983346,-3.6,2.86611571246965));
#22338=CARTESIAN_POINT('Origin',(39.31983346,0.,3.));
#22339=CARTESIAN_POINT('Origin',(39.31983346,0.,3.));
#22340=CARTESIAN_POINT('',(39.31983346,-0.0964364949201869,3.13388428753035));
#22341=CARTESIAN_POINT('Ctrl Pts',(39.31983346,-0.0964364949201871,3.13388428753035));
#22342=CARTESIAN_POINT('Ctrl Pts',(39.3210318640464,-0.103768349789617,
3.1286031720394));
#22343=CARTESIAN_POINT('Ctrl Pts',(39.3222741026686,-0.110552785281794,
3.12279245250977));
#22344=CARTESIAN_POINT('Ctrl Pts',(39.3263441031883,-0.131261405831701,
3.10208383195986));
#22345=CARTESIAN_POINT('Ctrl Pts',(39.3293775570573,-0.143943476007901,
3.08360021359466));
#22346=CARTESIAN_POINT('Ctrl Pts',(39.3336505364571,-0.160815615633796,
3.04297741500427));
#22347=CARTESIAN_POINT('Ctrl Pts',(39.3348334620742,-0.165,3.02082994033278));
#22348=CARTESIAN_POINT('Ctrl Pts',(39.3348334620742,-0.165,2.97917005966722));
#22349=CARTESIAN_POINT('Ctrl Pts',(39.3336505364571,-0.160815615633796,
2.95702258499573));
#22350=CARTESIAN_POINT('Ctrl Pts',(39.3293775570573,-0.143943476007901,
2.91639978640534));
#22351=CARTESIAN_POINT('Ctrl Pts',(39.3263441031883,-0.131261405831701,
2.89791616804014));
#22352=CARTESIAN_POINT('Ctrl Pts',(39.3222741026686,-0.110552785281793,
2.87720754749023));
#22353=CARTESIAN_POINT('Ctrl Pts',(39.3210318640464,-0.103768349789617,
2.8713968279606));
#22354=CARTESIAN_POINT('Ctrl Pts',(39.31983346,-0.0964364949201869,2.86611571246965));
#22355=CARTESIAN_POINT('',(39.31983346,-2.02066721859313E-17,3.165));
#22356=CARTESIAN_POINT('Origin',(39.31983346,0.,3.));
#22357=CARTESIAN_POINT('',(39.7298334620742,2.02066721859313E-17,3.165));
#22358=CARTESIAN_POINT('',(39.31983346,-2.02066721859313E-17,3.165));
#22359=CARTESIAN_POINT('Origin',(39.7298334620742,0.,3.));
#22360=CARTESIAN_POINT('',(39.31983346,0.0964364949201869,3.13388428753035));
#22361=CARTESIAN_POINT('Origin',(39.31983346,0.,3.));
#22362=CARTESIAN_POINT('Ctrl Pts',(39.31983346,0.0964364949201869,2.86611571246965));
#22363=CARTESIAN_POINT('Ctrl Pts',(39.3210318640464,0.103768349789617,2.8713968279606));
#22364=CARTESIAN_POINT('Ctrl Pts',(39.3222741026686,0.110552785281793,2.87720754749023));
#22365=CARTESIAN_POINT('Ctrl Pts',(39.3263441031883,0.1312614058317,2.89791616804014));
#22366=CARTESIAN_POINT('Ctrl Pts',(39.3293775570573,0.143943476007901,2.91639978640534));
#22367=CARTESIAN_POINT('Ctrl Pts',(39.3336505364571,0.160815615633796,2.95702258499573));
#22368=CARTESIAN_POINT('Ctrl Pts',(39.3348334620742,0.165,2.97917005966722));
#22369=CARTESIAN_POINT('Ctrl Pts',(39.3348334620742,0.165,3.02082994033278));
#22370=CARTESIAN_POINT('Ctrl Pts',(39.3336505364571,0.160815615633796,3.04297741500427));
#22371=CARTESIAN_POINT('Ctrl Pts',(39.3293775570573,0.143943476007901,3.08360021359466));
#22372=CARTESIAN_POINT('Ctrl Pts',(39.3263441031883,0.1312614058317,3.10208383195986));
#22373=CARTESIAN_POINT('Ctrl Pts',(39.3222741026686,0.110552785281793,3.12279245250977));
#22374=CARTESIAN_POINT('Ctrl Pts',(39.3210318640464,0.103768349789617,3.1286031720394));
#22375=CARTESIAN_POINT('Ctrl Pts',(39.31983346,0.0964364949201871,3.13388428753035));
#22376=CARTESIAN_POINT('Origin',(39.31983346,0.,3.));
#22377=CARTESIAN_POINT('',(39.31983346,-3.6,3.13388428753035));
#22378=CARTESIAN_POINT('Origin',(38.7298334620742,-3.6,3.));
#22379=CARTESIAN_POINT('',(38.1248334620742,-3.5,3.));
#22380=CARTESIAN_POINT('Origin',(38.7298334620742,-3.5,3.));
#22381=CARTESIAN_POINT('',(38.1248334620742,3.5,3.));
#22382=CARTESIAN_POINT('',(38.1248334620742,-3.6,3.));
#22383=CARTESIAN_POINT('Origin',(38.7298334620742,3.5,3.));
#22384=CARTESIAN_POINT('Origin',(39.7298334620742,3.5,2.));
#22385=CARTESIAN_POINT('',(39.7298334620742,3.5,2.));
#22386=CARTESIAN_POINT('',(37.7298334620742,3.5,2.));
#22387=CARTESIAN_POINT('',(39.7298334620742,3.5,2.));
#22388=CARTESIAN_POINT('',(37.7298334620742,3.5,4.3));
#22389=CARTESIAN_POINT('',(37.7298334620742,3.5,2.));
#22390=CARTESIAN_POINT('',(39.7298334620742,3.5,4.3));
#22391=CARTESIAN_POINT('',(39.7298334620742,3.5,4.3));
#22392=CARTESIAN_POINT('',(39.7298334620742,3.5,2.));
#22393=CARTESIAN_POINT('Origin',(39.7298334620742,-3.5,2.));
#22394=CARTESIAN_POINT('',(39.7298334620742,-3.5,2.));
#22395=CARTESIAN_POINT('',(39.7298334620742,-3.5,2.));
#22396=CARTESIAN_POINT('',(39.7298334620742,-3.5,4.3));
#22397=CARTESIAN_POINT('',(39.7298334620742,-3.5,4.3));
#22398=CARTESIAN_POINT('',(39.7298334620742,-3.5,2.));
#22399=CARTESIAN_POINT('Origin',(37.7298334620742,-3.5,2.));
#22400=CARTESIAN_POINT('',(37.7298334620742,-3.5,2.));
#22401=CARTESIAN_POINT('',(37.7298334620742,-3.5,2.));
#22402=CARTESIAN_POINT('',(37.7298334620742,-3.5,4.3));
#22403=CARTESIAN_POINT('',(37.7298334620742,-3.5,4.3));
#22404=CARTESIAN_POINT('',(37.7298334620742,-3.5,2.));
#22405=CARTESIAN_POINT('Origin',(37.7298334620742,3.5,2.));
#22406=CARTESIAN_POINT('',(37.7298334620742,3.5,2.));
#22407=CARTESIAN_POINT('',(37.7298334620742,3.5,4.3));
#22408=CARTESIAN_POINT('Origin',(38.7298334620742,0.,4.3));
#22409=CARTESIAN_POINT('Origin',(38.7298334620742,0.,2.));
#22410=CARTESIAN_POINT('',(0.,0.,0.));
#22411=CARTESIAN_POINT('Origin',(38.7298334620742,6.9,3.));
#22412=CARTESIAN_POINT('',(38.5648334620742,6.9,3.));
#22413=CARTESIAN_POINT('Origin',(38.7298334620742,6.9,3.));
#22414=CARTESIAN_POINT('',(38.5648334620742,8.5,3.));
#22415=CARTESIAN_POINT('',(38.5648334620742,6.9,3.));
#22416=CARTESIAN_POINT('Origin',(38.7298334620742,8.5,3.));
#22417=CARTESIAN_POINT('Origin',(38.7298334620742,6.9,3.));
#22418=CARTESIAN_POINT('Origin',(38.7298334620742,-6.1,3.));
#22419=CARTESIAN_POINT('',(38.5648334620742,-6.,3.));
#22420=CARTESIAN_POINT('Origin',(38.7298334620742,-6.,3.));
#22421=CARTESIAN_POINT('',(38.5648334620742,-4.4,3.));
#22422=CARTESIAN_POINT('',(38.5648334620742,-6.1,3.));
#22423=CARTESIAN_POINT('Origin',(38.7298334620742,-4.4,3.));
#22424=CARTESIAN_POINT('Origin',(38.7298334620742,-4.4,3.));
#22425=CARTESIAN_POINT('Origin',(38.7298334620742,-6.,3.));
#22426=CARTESIAN_POINT('',(38.1298334620742,8.5,3.));
#22427=CARTESIAN_POINT('Origin',(38.7298334620742,8.5,3.));
#22428=CARTESIAN_POINT('',(38.1298334620742,-6.,3.));
#22429=CARTESIAN_POINT('',(38.1298334620742,-6.,3.));
#22430=CARTESIAN_POINT('Origin',(38.7298334620742,-6.,3.));
#22431=CARTESIAN_POINT('Origin',(38.7298334620742,8.5,3.));
#22432=CARTESIAN_POINT('Origin',(38.7298334620742,-6.,3.));
#22433=CARTESIAN_POINT('',(0.,0.,0.));
#22434=CARTESIAN_POINT('Origin',(38.7298334620742,-6.2,3.));
#22435=CARTESIAN_POINT('',(38.5048334620742,-6.,3.));
#22436=CARTESIAN_POINT('Origin',(38.7298334620742,-6.,3.));
#22437=CARTESIAN_POINT('',(38.5048334620742,-6.2,3.));
#22438=CARTESIAN_POINT('',(38.5048334620742,-6.2,3.));
#22439=CARTESIAN_POINT('Origin',(38.7298334620742,-6.2,3.));
#22440=CARTESIAN_POINT('Origin',(38.7298334620742,-6.2,3.));
#22441=CARTESIAN_POINT('',(37.7298334620742,-6.,3.));
#22442=CARTESIAN_POINT('Origin',(38.7298334620742,-6.,3.));
#22443=CARTESIAN_POINT('',(37.7298334620742,-6.2,3.));
#22444=CARTESIAN_POINT('',(37.7298334620742,-6.2,3.));
#22445=CARTESIAN_POINT('Origin',(38.7298334620742,-6.2,3.));
#22446=CARTESIAN_POINT('Origin',(38.7298334620742,-6.,3.));
#22447=CARTESIAN_POINT('Origin',(38.7298334620742,-6.2,3.));
#22448=CARTESIAN_POINT('',(0.,0.,0.));
#22449=CARTESIAN_POINT('Origin',(38.7298334620742,8.5,3.));
#22450=CARTESIAN_POINT('',(38.5048334620742,8.7,3.));
#22451=CARTESIAN_POINT('Origin',(38.7298334620742,8.7,3.));
#22452=CARTESIAN_POINT('',(38.5048334620742,8.5,3.));
#22453=CARTESIAN_POINT('',(38.5048334620742,8.5,3.));
#22454=CARTESIAN_POINT('Origin',(38.7298334620742,8.5,3.));
#22455=CARTESIAN_POINT('Origin',(38.7298334620742,8.5,3.));
#22456=CARTESIAN_POINT('',(37.7298334620742,8.7,3.));
#22457=CARTESIAN_POINT('Origin',(38.7298334620742,8.7,3.));
#22458=CARTESIAN_POINT('',(37.7298334620742,8.5,3.));
#22459=CARTESIAN_POINT('',(37.7298334620742,8.5,3.));
#22460=CARTESIAN_POINT('Origin',(38.7298334620742,8.5,3.));
#22461=CARTESIAN_POINT('Origin',(38.7298334620742,8.7,3.));
#22462=CARTESIAN_POINT('Origin',(38.7298334620742,8.5,3.));
#22463=CARTESIAN_POINT('',(0.,0.,0.));
#22464=CARTESIAN_POINT('Origin',(38.7298334620742,-6.,3.));
#22465=CARTESIAN_POINT('',(38.1248334620742,-5.5,3.));
#22466=CARTESIAN_POINT('Origin',(38.7298334620742,-5.5,3.));
#22467=CARTESIAN_POINT('',(38.1248334620742,-6.,3.));
#22468=CARTESIAN_POINT('',(38.1248334620742,-6.,3.));
#22469=CARTESIAN_POINT('Origin',(38.7298334620742,-6.,3.));
#22470=CARTESIAN_POINT('Origin',(38.7298334620742,-6.,3.));
#22471=CARTESIAN_POINT('',(37.9298334620742,-5.5,3.));
#22472=CARTESIAN_POINT('Origin',(38.7298334620742,-5.5,3.));
#22473=CARTESIAN_POINT('',(37.9298334620742,-6.,3.));
#22474=CARTESIAN_POINT('',(37.9298334620742,-6.,3.));
#22475=CARTESIAN_POINT('Origin',(38.7298334620742,-6.,3.));
#22476=CARTESIAN_POINT('Origin',(38.7298334620742,-5.5,3.));
#22477=CARTESIAN_POINT('Origin',(38.7298334620742,-6.,3.));
#22478=CARTESIAN_POINT('',(0.,0.,0.));
#22479=CARTESIAN_POINT('Origin',(38.7298334620742,-4.5,3.));
#22480=CARTESIAN_POINT('',(38.1248334620742,-3.5,3.));
#22481=CARTESIAN_POINT('Origin',(38.7298334620742,-3.5,3.));
#22482=CARTESIAN_POINT('',(38.1248334620742,-4.5,3.));
#22483=CARTESIAN_POINT('',(38.1248334620742,-4.5,3.));
#22484=CARTESIAN_POINT('Origin',(38.7298334620742,-4.5,3.));
#22485=CARTESIAN_POINT('Origin',(38.7298334620742,-4.5,3.));
#22486=CARTESIAN_POINT('',(37.9298334620742,-3.5,3.));
#22487=CARTESIAN_POINT('Origin',(38.7298334620742,-3.5,3.));
#22488=CARTESIAN_POINT('',(37.9298334620742,-4.5,3.));
#22489=CARTESIAN_POINT('',(37.9298334620742,-4.5,3.));
#22490=CARTESIAN_POINT('Origin',(38.7298334620742,-4.5,3.));
#22491=CARTESIAN_POINT('Origin',(38.7298334620742,-3.5,3.));
#22492=CARTESIAN_POINT('Origin',(38.7298334620742,-4.5,3.));
#22493=CARTESIAN_POINT('',(0.,0.,0.));
#22494=CARTESIAN_POINT('Origin',(38.7298334620742,3.5,3.));
#22495=CARTESIAN_POINT('',(38.1248334620742,7.,3.));
#22496=CARTESIAN_POINT('Origin',(38.7298334620742,7.,3.));
#22497=CARTESIAN_POINT('',(38.1248334620742,3.5,3.));
#22498=CARTESIAN_POINT('',(38.1248334620742,3.5,3.));
#22499=CARTESIAN_POINT('Origin',(38.7298334620742,3.5,3.));
#22500=CARTESIAN_POINT('Origin',(38.7298334620742,3.5,3.));
#22501=CARTESIAN_POINT('',(37.9298334620742,7.,3.));
#22502=CARTESIAN_POINT('Origin',(38.7298334620742,7.,3.));
#22503=CARTESIAN_POINT('',(37.9298334620742,3.5,3.));
#22504=CARTESIAN_POINT('',(37.9298334620742,3.5,3.));
#22505=CARTESIAN_POINT('Origin',(38.7298334620742,3.5,3.));
#22506=CARTESIAN_POINT('Origin',(38.7298334620742,7.,3.));
#22507=CARTESIAN_POINT('Origin',(38.7298334620742,3.5,3.));
#22508=CARTESIAN_POINT('',(0.,0.,0.));
#22509=CARTESIAN_POINT('Origin',(38.7298334620742,8.,3.));
#22510=CARTESIAN_POINT('',(38.1248334620742,8.5,3.));
#22511=CARTESIAN_POINT('Origin',(38.7298334620742,8.5,3.));
#22512=CARTESIAN_POINT('',(38.1248334620742,8.,3.));
#22513=CARTESIAN_POINT('',(38.1248334620742,8.,3.));
#22514=CARTESIAN_POINT('Origin',(38.7298334620742,8.,3.));
#22515=CARTESIAN_POINT('Origin',(38.7298334620742,8.,3.));
#22516=CARTESIAN_POINT('',(37.9298334620742,8.5,3.));
#22517=CARTESIAN_POINT('Origin',(38.7298334620742,8.5,3.));
#22518=CARTESIAN_POINT('',(37.9298334620742,8.,3.));
#22519=CARTESIAN_POINT('',(37.9298334620742,8.,3.));
#22520=CARTESIAN_POINT('Origin',(38.7298334620742,8.,3.));
#22521=CARTESIAN_POINT('Origin',(38.7298334620742,8.5,3.));
#22522=CARTESIAN_POINT('Origin',(38.7298334620742,8.,3.));
#22523=CARTESIAN_POINT('',(0.,0.,0.));
#22524=CARTESIAN_POINT('',(0.,0.,0.));
#22525=CARTESIAN_POINT('Origin',(36.92983346,0.,16.));
#22526=CARTESIAN_POINT('',(37.0298334620742,-7.9602041944578E-17,16.65));
#22527=CARTESIAN_POINT('Origin',(37.0298334620742,0.,16.));
#22528=CARTESIAN_POINT('',(40.4298334620742,7.9602041944578E-17,16.65));
#22529=CARTESIAN_POINT('',(36.92983346,-7.9602041944578E-17,16.65));
#22530=CARTESIAN_POINT('Origin',(40.4298334620742,0.,16.));
#22531=CARTESIAN_POINT('Origin',(36.92983346,-3.,16.));
#22532=CARTESIAN_POINT('',(37.0298334620742,-3.,17.05));
#22533=CARTESIAN_POINT('Origin',(37.0298334620742,-3.,16.));
#22534=CARTESIAN_POINT('',(40.4298334620742,-3.,17.05));
#22535=CARTESIAN_POINT('',(36.92983346,-3.,17.05));
#22536=CARTESIAN_POINT('Origin',(40.4298334620742,-3.,16.));
#22537=CARTESIAN_POINT('Origin',(36.92983346,3.,16.));
#22538=CARTESIAN_POINT('',(37.0298334620742,3.,17.05));
#22539=CARTESIAN_POINT('Origin',(37.0298334620742,3.,16.));
#22540=CARTESIAN_POINT('',(40.4298334620742,3.,17.05));
#22541=CARTESIAN_POINT('',(36.92983346,3.,17.05));
#22542=CARTESIAN_POINT('Origin',(40.4298334620742,3.,16.));
#22543=CARTESIAN_POINT('Origin',(40.4298334620742,4.7,14.3));
#22544=CARTESIAN_POINT('',(40.4298334620742,4.7,14.3));
#22545=CARTESIAN_POINT('',(37.0298334620742,4.7,14.3));
#22546=CARTESIAN_POINT('',(40.4298334620742,4.7,14.3));
#22547=CARTESIAN_POINT('',(37.0298334620742,4.7,17.7));
#22548=CARTESIAN_POINT('',(37.0298334620742,4.7,14.3));
#22549=CARTESIAN_POINT('',(40.4298334620742,4.7,17.7));
#22550=CARTESIAN_POINT('',(40.4298334620742,4.7,17.7));
#22551=CARTESIAN_POINT('',(40.4298334620742,4.7,14.3));
#22552=CARTESIAN_POINT('Origin',(40.4298334620742,-4.3,14.3));
#22553=CARTESIAN_POINT('',(40.4298334620742,-4.3,14.3));
#22554=CARTESIAN_POINT('',(40.4298334620742,-4.3,14.3));
#22555=CARTESIAN_POINT('',(40.4298334620742,-4.3,17.7));
#22556=CARTESIAN_POINT('',(40.4298334620742,-4.3,17.7));
#22557=CARTESIAN_POINT('',(40.4298334620742,-4.3,14.3));
#22558=CARTESIAN_POINT('Origin',(37.0298334620742,-4.3,14.3));
#22559=CARTESIAN_POINT('',(37.0298334620742,-4.3,14.3));
#22560=CARTESIAN_POINT('',(37.0298334620742,-4.3,14.3));
#22561=CARTESIAN_POINT('',(37.0298334620742,-4.3,17.7));
#22562=CARTESIAN_POINT('',(37.0298334620742,-4.3,17.7));
#22563=CARTESIAN_POINT('',(37.0298334620742,-4.3,14.3));
#22564=CARTESIAN_POINT('Origin',(37.0298334620742,4.7,14.3));
#22565=CARTESIAN_POINT('',(37.0298334620742,4.7,14.3));
#22566=CARTESIAN_POINT('',(37.0298334620742,4.7,17.7));
#22567=CARTESIAN_POINT('Origin',(38.7298334620742,0.2,17.7));
#22568=CARTESIAN_POINT('Origin',(38.7298334620742,0.2,14.3));
#22569=CARTESIAN_POINT('',(0.,0.,0.));
#22570=CARTESIAN_POINT('Origin',(37.02983346,3.,16.));
#22571=CARTESIAN_POINT('',(37.22983346,3.,17.04));
#22572=CARTESIAN_POINT('Origin',(37.22983346,3.,16.));
#22573=CARTESIAN_POINT('',(37.02983346,3.,17.04));
#22574=CARTESIAN_POINT('',(37.02983346,3.,17.04));
#22575=CARTESIAN_POINT('Origin',(37.02983346,3.,16.));
#22576=CARTESIAN_POINT('Origin',(37.22983346,3.,16.));
#22577=CARTESIAN_POINT('',(37.22983346,3.,16.8));
#22578=CARTESIAN_POINT('Origin',(37.22983346,3.,16.));
#22579=CARTESIAN_POINT('Origin',(37.02983346,-3.,16.));
#22580=CARTESIAN_POINT('',(37.22983346,-3.,17.04));
#22581=CARTESIAN_POINT('Origin',(37.22983346,-3.,16.));
#22582=CARTESIAN_POINT('',(37.02983346,-3.,17.04));
#22583=CARTESIAN_POINT('',(37.02983346,-3.,17.04));
#22584=CARTESIAN_POINT('Origin',(37.02983346,-3.,16.));
#22585=CARTESIAN_POINT('Origin',(37.22983346,-3.,16.));
#22586=CARTESIAN_POINT('',(37.22983346,-3.,16.8));
#22587=CARTESIAN_POINT('Origin',(37.22983346,-3.,16.));
#22588=CARTESIAN_POINT('Origin',(36.72983346,0.,16.));
#22589=CARTESIAN_POINT('',(36.82983346,-7.9602041944578E-17,16.65));
#22590=CARTESIAN_POINT('Origin',(36.82983346,0.,16.));
#22591=CARTESIAN_POINT('',(37.02983346,7.9602041944578E-17,16.65));
#22592=CARTESIAN_POINT('',(36.72983346,-7.9602041944578E-17,16.65));
#22593=CARTESIAN_POINT('Origin',(37.02983346,0.,16.));
#22594=CARTESIAN_POINT('Origin',(36.72983346,-3.,16.));
#22595=CARTESIAN_POINT('',(36.82983346,-3.,16.8));
#22596=CARTESIAN_POINT('Origin',(36.82983346,-3.,16.));
#22597=CARTESIAN_POINT('',(36.72983346,-3.,16.8));
#22598=CARTESIAN_POINT('Origin',(36.72983346,3.,16.));
#22599=CARTESIAN_POINT('',(36.82983346,3.,16.8));
#22600=CARTESIAN_POINT('Origin',(36.82983346,3.,16.));
#22601=CARTESIAN_POINT('',(36.72983346,3.,16.8));
#22602=CARTESIAN_POINT('Origin',(36.82983346,4.7,17.7));
#22603=CARTESIAN_POINT('',(36.82983346,4.7,17.7));
#22604=CARTESIAN_POINT('',(36.82983346,-4.3,17.7));
#22605=CARTESIAN_POINT('',(36.82983346,4.7,17.7));
#22606=CARTESIAN_POINT('',(37.02983346,-4.3,17.7));
#22607=CARTESIAN_POINT('',(36.82983346,-4.3,17.7));
#22608=CARTESIAN_POINT('',(37.02983346,4.7,17.7));
#22609=CARTESIAN_POINT('',(37.02983346,4.7,17.7));
#22610=CARTESIAN_POINT('',(36.82983346,4.7,17.7));
#22611=CARTESIAN_POINT('Origin',(36.82983346,4.7,14.3));
#22612=CARTESIAN_POINT('',(36.82983346,4.7,14.3));
#22613=CARTESIAN_POINT('',(36.82983346,4.7,14.3));
#22614=CARTESIAN_POINT('',(37.02983346,4.7,14.3));
#22615=CARTESIAN_POINT('',(37.02983346,4.7,14.3));
#22616=CARTESIAN_POINT('',(36.82983346,4.7,14.3));
#22617=CARTESIAN_POINT('Origin',(36.82983346,-4.3,14.3));
#22618=CARTESIAN_POINT('',(36.82983346,-4.3,14.3));
#22619=CARTESIAN_POINT('',(36.82983346,-4.3,14.3));
#22620=CARTESIAN_POINT('',(37.02983346,-4.3,14.3));
#22621=CARTESIAN_POINT('',(37.02983346,-4.3,14.3));
#22622=CARTESIAN_POINT('',(36.82983346,-4.3,14.3));
#22623=CARTESIAN_POINT('Origin',(36.82983346,-4.3,17.7));
#22624=CARTESIAN_POINT('',(36.82983346,-4.3,17.7));
#22625=CARTESIAN_POINT('',(37.02983346,-4.3,17.7));
#22626=CARTESIAN_POINT('Origin',(37.02983346,0.2,16.));
#22627=CARTESIAN_POINT('Origin',(36.82983346,0.2,16.));
#22628=CARTESIAN_POINT('',(0.,0.,0.));
#22629=CARTESIAN_POINT('Origin',(40.22983346,3.,16.));
#22630=CARTESIAN_POINT('',(40.42983346,3.,17.04));
#22631=CARTESIAN_POINT('Origin',(40.42983346,3.,16.));
#22632=CARTESIAN_POINT('',(40.22983346,3.,17.04));
#22633=CARTESIAN_POINT('',(40.22983346,3.,17.04));
#22634=CARTESIAN_POINT('Origin',(40.22983346,3.,16.));
#22635=CARTESIAN_POINT('Origin',(40.22983346,3.,16.));
#22636=CARTESIAN_POINT('',(40.22983346,3.,16.8));
#22637=CARTESIAN_POINT('Origin',(40.22983346,3.,16.));
#22638=CARTESIAN_POINT('Origin',(40.22983346,-3.,16.));
#22639=CARTESIAN_POINT('',(40.42983346,-3.,17.04));
#22640=CARTESIAN_POINT('Origin',(40.42983346,-3.,16.));
#22641=CARTESIAN_POINT('',(40.22983346,-3.,17.04));
#22642=CARTESIAN_POINT('',(40.22983346,-3.,17.04));
#22643=CARTESIAN_POINT('Origin',(40.22983346,-3.,16.));
#22644=CARTESIAN_POINT('Origin',(40.22983346,-3.,16.));
#22645=CARTESIAN_POINT('',(40.22983346,-3.,16.8));
#22646=CARTESIAN_POINT('Origin',(40.22983346,-3.,16.));
#22647=CARTESIAN_POINT('Origin',(40.32983346,0.,16.));
#22648=CARTESIAN_POINT('',(40.42983346,-7.9602041944578E-17,16.65));
#22649=CARTESIAN_POINT('Origin',(40.42983346,0.,16.));
#22650=CARTESIAN_POINT('',(40.62983346,7.9602041944578E-17,16.65));
#22651=CARTESIAN_POINT('',(40.32983346,-7.9602041944578E-17,16.65));
#22652=CARTESIAN_POINT('Origin',(40.62983346,0.,16.));
#22653=CARTESIAN_POINT('Origin',(40.32983346,-3.,16.));
#22654=CARTESIAN_POINT('',(40.62983346,-3.,16.8));
#22655=CARTESIAN_POINT('',(40.32983346,-3.,16.8));
#22656=CARTESIAN_POINT('Origin',(40.62983346,-3.,16.));
#22657=CARTESIAN_POINT('Origin',(40.32983346,3.,16.));
#22658=CARTESIAN_POINT('',(40.62983346,3.,16.8));
#22659=CARTESIAN_POINT('',(40.32983346,3.,16.8));
#22660=CARTESIAN_POINT('Origin',(40.62983346,3.,16.));
#22661=CARTESIAN_POINT('Origin',(40.42983346,4.7,17.7));
#22662=CARTESIAN_POINT('',(40.42983346,4.7,17.7));
#22663=CARTESIAN_POINT('',(40.42983346,-4.3,17.7));
#22664=CARTESIAN_POINT('',(40.42983346,4.7,17.7));
#22665=CARTESIAN_POINT('',(40.62983346,-4.3,17.7));
#22666=CARTESIAN_POINT('',(40.42983346,-4.3,17.7));
#22667=CARTESIAN_POINT('',(40.62983346,4.7,17.7));
#22668=CARTESIAN_POINT('',(40.62983346,4.7,17.7));
#22669=CARTESIAN_POINT('',(40.42983346,4.7,17.7));
#22670=CARTESIAN_POINT('Origin',(40.42983346,4.7,14.3));
#22671=CARTESIAN_POINT('',(40.42983346,4.7,14.3));
#22672=CARTESIAN_POINT('',(40.42983346,4.7,14.3));
#22673=CARTESIAN_POINT('',(40.62983346,4.7,14.3));
#22674=CARTESIAN_POINT('',(40.62983346,4.7,14.3));
#22675=CARTESIAN_POINT('',(40.42983346,4.7,14.3));
#22676=CARTESIAN_POINT('Origin',(40.42983346,-4.3,14.3));
#22677=CARTESIAN_POINT('',(40.42983346,-4.3,14.3));
#22678=CARTESIAN_POINT('',(40.42983346,-4.3,14.3));
#22679=CARTESIAN_POINT('',(40.62983346,-4.3,14.3));
#22680=CARTESIAN_POINT('',(40.62983346,-4.3,14.3));
#22681=CARTESIAN_POINT('',(40.42983346,-4.3,14.3));
#22682=CARTESIAN_POINT('Origin',(40.42983346,-4.3,17.7));
#22683=CARTESIAN_POINT('',(40.42983346,-4.3,17.7));
#22684=CARTESIAN_POINT('',(40.62983346,-4.3,17.7));
#22685=CARTESIAN_POINT('Origin',(40.62983346,0.2,16.));
#22686=CARTESIAN_POINT('Origin',(40.42983346,0.2,16.));
#22687=CARTESIAN_POINT('',(0.,0.,0.));
#22688=CARTESIAN_POINT('Origin',(39.31983346,0.,13.));
#22689=CARTESIAN_POINT('',(39.31983346,-0.0964364949201854,12.8661157124697));
#22690=CARTESIAN_POINT('',(39.31983346,0.0964364949201854,12.8661157124697));
#22691=CARTESIAN_POINT('',(39.31983346,-3.6,12.8661157124697));
#22692=CARTESIAN_POINT('Origin',(39.31983346,0.,13.));
#22693=CARTESIAN_POINT('Origin',(39.31983346,0.,13.));
#22694=CARTESIAN_POINT('',(39.31983346,-0.0964364949201854,13.1338842875303));
#22695=CARTESIAN_POINT('Ctrl Pts',(39.31983346,-0.0964364949201853,13.1338842875303));
#22696=CARTESIAN_POINT('Ctrl Pts',(39.3210318640464,-0.103768349789616,
13.1286031720394));
#22697=CARTESIAN_POINT('Ctrl Pts',(39.3222741026686,-0.110552785281792,
13.1227924525098));
#22698=CARTESIAN_POINT('Ctrl Pts',(39.3263441031883,-0.1312614058317,13.1020838319599));
#22699=CARTESIAN_POINT('Ctrl Pts',(39.3293775570573,-0.143943476007901,
13.0836002135947));
#22700=CARTESIAN_POINT('Ctrl Pts',(39.3336505364571,-0.160815615633794,
13.0429774150043));
#22701=CARTESIAN_POINT('Ctrl Pts',(39.3348334620742,-0.164999999999999,
13.0208299403328));
#22702=CARTESIAN_POINT('Ctrl Pts',(39.3348334620742,-0.164999999999999,
12.9791700596672));
#22703=CARTESIAN_POINT('Ctrl Pts',(39.3336505364571,-0.160815615633794,
12.9570225849957));
#22704=CARTESIAN_POINT('Ctrl Pts',(39.3293775570573,-0.143943476007901,
12.9163997864053));
#22705=CARTESIAN_POINT('Ctrl Pts',(39.3263441031883,-0.1312614058317,12.8979161680401));
#22706=CARTESIAN_POINT('Ctrl Pts',(39.3222741026686,-0.110552785281793,
12.8772075474902));
#22707=CARTESIAN_POINT('Ctrl Pts',(39.3210318640464,-0.103768349789615,
12.8713968279606));
#22708=CARTESIAN_POINT('Ctrl Pts',(39.31983346,-0.0964364949201854,12.8661157124697));
#22709=CARTESIAN_POINT('',(39.31983346,-2.02066721859312E-17,13.165));
#22710=CARTESIAN_POINT('Origin',(39.31983346,0.,13.));
#22711=CARTESIAN_POINT('',(39.7298334620742,2.02066721859312E-17,13.165));
#22712=CARTESIAN_POINT('',(39.31983346,-2.02066721859312E-17,13.165));
#22713=CARTESIAN_POINT('Origin',(39.7298334620742,0.,13.));
#22714=CARTESIAN_POINT('',(39.31983346,0.0964364949201854,13.1338842875303));
#22715=CARTESIAN_POINT('Origin',(39.31983346,0.,13.));
#22716=CARTESIAN_POINT('Ctrl Pts',(39.31983346,0.0964364949201854,12.8661157124697));
#22717=CARTESIAN_POINT('Ctrl Pts',(39.3210318640464,0.103768349789616,12.8713968279606));
#22718=CARTESIAN_POINT('Ctrl Pts',(39.3222741026686,0.110552785281793,12.8772075474902));
#22719=CARTESIAN_POINT('Ctrl Pts',(39.3263441031883,0.1312614058317,12.8979161680401));
#22720=CARTESIAN_POINT('Ctrl Pts',(39.3293775570573,0.143943476007901,12.9163997864053));
#22721=CARTESIAN_POINT('Ctrl Pts',(39.3336505364571,0.160815615633794,12.9570225849957));
#22722=CARTESIAN_POINT('Ctrl Pts',(39.3348334620742,0.164999999999999,12.9791700596672));
#22723=CARTESIAN_POINT('Ctrl Pts',(39.3348334620742,0.164999999999999,13.0208299403328));
#22724=CARTESIAN_POINT('Ctrl Pts',(39.3336505364571,0.160815615633794,13.0429774150043));
#22725=CARTESIAN_POINT('Ctrl Pts',(39.3293775570573,0.143943476007901,13.0836002135947));
#22726=CARTESIAN_POINT('Ctrl Pts',(39.3263441031883,0.1312614058317,13.1020838319599));
#22727=CARTESIAN_POINT('Ctrl Pts',(39.3222741026686,0.110552785281792,13.1227924525098));
#22728=CARTESIAN_POINT('Ctrl Pts',(39.3210318640464,0.103768349789616,13.1286031720394));
#22729=CARTESIAN_POINT('Ctrl Pts',(39.31983346,0.0964364949201853,13.1338842875303));
#22730=CARTESIAN_POINT('Origin',(39.31983346,0.,13.));
#22731=CARTESIAN_POINT('',(39.31983346,-3.6,13.1338842875303));
#22732=CARTESIAN_POINT('Origin',(38.7298334620742,-3.6,13.));
#22733=CARTESIAN_POINT('',(38.1248334620742,-3.5,13.));
#22734=CARTESIAN_POINT('Origin',(38.7298334620742,-3.5,13.));
#22735=CARTESIAN_POINT('',(38.1248334620742,3.5,13.));
#22736=CARTESIAN_POINT('',(38.1248334620742,-3.6,13.));
#22737=CARTESIAN_POINT('Origin',(38.7298334620742,3.5,13.));
#22738=CARTESIAN_POINT('Origin',(39.7298334620742,3.5,12.));
#22739=CARTESIAN_POINT('',(39.7298334620742,3.5,12.));
#22740=CARTESIAN_POINT('',(37.7298334620742,3.5,12.));
#22741=CARTESIAN_POINT('',(39.7298334620742,3.5,12.));
#22742=CARTESIAN_POINT('',(37.7298334620742,3.5,14.3));
#22743=CARTESIAN_POINT('',(37.7298334620742,3.5,12.));
#22744=CARTESIAN_POINT('',(39.7298334620742,3.5,14.3));
#22745=CARTESIAN_POINT('',(39.7298334620742,3.5,14.3));
#22746=CARTESIAN_POINT('',(39.7298334620742,3.5,12.));
#22747=CARTESIAN_POINT('Origin',(39.7298334620742,-3.5,12.));
#22748=CARTESIAN_POINT('',(39.7298334620742,-3.5,12.));
#22749=CARTESIAN_POINT('',(39.7298334620742,-3.5,12.));
#22750=CARTESIAN_POINT('',(39.7298334620742,-3.5,14.3));
#22751=CARTESIAN_POINT('',(39.7298334620742,-3.5,14.3));
#22752=CARTESIAN_POINT('',(39.7298334620742,-3.5,12.));
#22753=CARTESIAN_POINT('Origin',(37.7298334620742,-3.5,12.));
#22754=CARTESIAN_POINT('',(37.7298334620742,-3.5,12.));
#22755=CARTESIAN_POINT('',(37.7298334620742,-3.5,12.));
#22756=CARTESIAN_POINT('',(37.7298334620742,-3.5,14.3));
#22757=CARTESIAN_POINT('',(37.7298334620742,-3.5,14.3));
#22758=CARTESIAN_POINT('',(37.7298334620742,-3.5,12.));
#22759=CARTESIAN_POINT('Origin',(37.7298334620742,3.5,12.));
#22760=CARTESIAN_POINT('',(37.7298334620742,3.5,12.));
#22761=CARTESIAN_POINT('',(37.7298334620742,3.5,14.3));
#22762=CARTESIAN_POINT('Origin',(38.7298334620742,0.,14.3));
#22763=CARTESIAN_POINT('Origin',(38.7298334620742,0.,12.));
#22764=CARTESIAN_POINT('',(0.,0.,0.));
#22765=CARTESIAN_POINT('Origin',(38.7298334620742,4.9,13.));
#22766=CARTESIAN_POINT('',(38.5648334620742,4.9,13.));
#22767=CARTESIAN_POINT('Origin',(38.7298334620742,4.9,13.));
#22768=CARTESIAN_POINT('',(38.5648334620742,6.5,13.));
#22769=CARTESIAN_POINT('',(38.5648334620742,4.9,13.));
#22770=CARTESIAN_POINT('Origin',(38.7298334620742,6.5,13.));
#22771=CARTESIAN_POINT('Origin',(38.7298334620742,4.9,13.));
#22772=CARTESIAN_POINT('Origin',(38.7298334620742,-7.6,13.));
#22773=CARTESIAN_POINT('',(38.5648334620742,-7.5,13.));
#22774=CARTESIAN_POINT('Origin',(38.7298334620742,-7.5,13.));
#22775=CARTESIAN_POINT('',(38.5648334620742,-5.9,13.));
#22776=CARTESIAN_POINT('',(38.5648334620742,-7.6,13.));
#22777=CARTESIAN_POINT('Origin',(38.7298334620742,-5.9,13.));
#22778=CARTESIAN_POINT('Origin',(38.7298334620742,-5.9,13.));
#22779=CARTESIAN_POINT('Origin',(38.7298334620742,-7.5,13.));
#22780=CARTESIAN_POINT('',(38.1298334620742,6.5,13.));
#22781=CARTESIAN_POINT('Origin',(38.7298334620742,6.5,13.));
#22782=CARTESIAN_POINT('',(38.1298334620742,-7.5,13.));
#22783=CARTESIAN_POINT('',(38.1298334620742,-7.5,13.));
#22784=CARTESIAN_POINT('Origin',(38.7298334620742,-7.5,13.));
#22785=CARTESIAN_POINT('Origin',(38.7298334620742,6.5,13.));
#22786=CARTESIAN_POINT('Origin',(38.7298334620742,-7.5,13.));
#22787=CARTESIAN_POINT('',(0.,0.,0.));
#22788=CARTESIAN_POINT('Origin',(38.7298334620742,-7.7,13.));
#22789=CARTESIAN_POINT('',(38.5048334620742,-7.5,13.));
#22790=CARTESIAN_POINT('Origin',(38.7298334620742,-7.5,13.));
#22791=CARTESIAN_POINT('',(38.5048334620742,-7.7,13.));
#22792=CARTESIAN_POINT('',(38.5048334620742,-7.7,13.));
#22793=CARTESIAN_POINT('Origin',(38.7298334620742,-7.7,13.));
#22794=CARTESIAN_POINT('Origin',(38.7298334620742,-7.7,13.));
#22795=CARTESIAN_POINT('',(37.7298334620742,-7.5,13.));
#22796=CARTESIAN_POINT('Origin',(38.7298334620742,-7.5,13.));
#22797=CARTESIAN_POINT('',(37.7298334620742,-7.7,13.));
#22798=CARTESIAN_POINT('',(37.7298334620742,-7.7,13.));
#22799=CARTESIAN_POINT('Origin',(38.7298334620742,-7.7,13.));
#22800=CARTESIAN_POINT('Origin',(38.7298334620742,-7.5,13.));
#22801=CARTESIAN_POINT('Origin',(38.7298334620742,-7.7,13.));
#22802=CARTESIAN_POINT('',(0.,0.,0.));
#22803=CARTESIAN_POINT('Origin',(38.7298334620742,6.5,13.));
#22804=CARTESIAN_POINT('',(38.5048334620742,6.7,13.));
#22805=CARTESIAN_POINT('Origin',(38.7298334620742,6.7,13.));
#22806=CARTESIAN_POINT('',(38.5048334620742,6.5,13.));
#22807=CARTESIAN_POINT('',(38.5048334620742,6.5,13.));
#22808=CARTESIAN_POINT('Origin',(38.7298334620742,6.5,13.));
#22809=CARTESIAN_POINT('Origin',(38.7298334620742,6.5,13.));
#22810=CARTESIAN_POINT('',(37.7298334620742,6.7,13.));
#22811=CARTESIAN_POINT('Origin',(38.7298334620742,6.7,13.));
#22812=CARTESIAN_POINT('',(37.7298334620742,6.5,13.));
#22813=CARTESIAN_POINT('',(37.7298334620742,6.5,13.));
#22814=CARTESIAN_POINT('Origin',(38.7298334620742,6.5,13.));
#22815=CARTESIAN_POINT('Origin',(38.7298334620742,6.7,13.));
#22816=CARTESIAN_POINT('Origin',(38.7298334620742,6.5,13.));
#22817=CARTESIAN_POINT('',(0.,0.,0.));
#22818=CARTESIAN_POINT('Origin',(38.7298334620742,-7.5,13.));
#22819=CARTESIAN_POINT('',(38.1248334620742,-7.,13.));
#22820=CARTESIAN_POINT('Origin',(38.7298334620742,-7.,13.));
#22821=CARTESIAN_POINT('',(38.1248334620742,-7.5,13.));
#22822=CARTESIAN_POINT('',(38.1248334620742,-7.5,13.));
#22823=CARTESIAN_POINT('Origin',(38.7298334620742,-7.5,13.));
#22824=CARTESIAN_POINT('Origin',(38.7298334620742,-7.5,13.));
#22825=CARTESIAN_POINT('',(37.9298334620742,-7.,13.));
#22826=CARTESIAN_POINT('Origin',(38.7298334620742,-7.,13.));
#22827=CARTESIAN_POINT('',(37.9298334620742,-7.5,13.));
#22828=CARTESIAN_POINT('',(37.9298334620742,-7.5,13.));
#22829=CARTESIAN_POINT('Origin',(38.7298334620742,-7.5,13.));
#22830=CARTESIAN_POINT('Origin',(38.7298334620742,-7.,13.));
#22831=CARTESIAN_POINT('Origin',(38.7298334620742,-7.5,13.));
#22832=CARTESIAN_POINT('',(0.,0.,0.));
#22833=CARTESIAN_POINT('Origin',(38.7298334620742,-6.,13.));
#22834=CARTESIAN_POINT('',(38.1248334620742,-3.5,13.));
#22835=CARTESIAN_POINT('Origin',(38.7298334620742,-3.5,13.));
#22836=CARTESIAN_POINT('',(38.1248334620742,-6.,13.));
#22837=CARTESIAN_POINT('',(38.1248334620742,-6.,13.));
#22838=CARTESIAN_POINT('Origin',(38.7298334620742,-6.,13.));
#22839=CARTESIAN_POINT('Origin',(38.7298334620742,-6.,13.));
#22840=CARTESIAN_POINT('',(37.9298334620742,-3.5,13.));
#22841=CARTESIAN_POINT('Origin',(38.7298334620742,-3.5,13.));
#22842=CARTESIAN_POINT('',(37.9298334620742,-6.,13.));
#22843=CARTESIAN_POINT('',(37.9298334620742,-6.,13.));
#22844=CARTESIAN_POINT('Origin',(38.7298334620742,-6.,13.));
#22845=CARTESIAN_POINT('Origin',(38.7298334620742,-3.5,13.));
#22846=CARTESIAN_POINT('Origin',(38.7298334620742,-6.,13.));
#22847=CARTESIAN_POINT('',(0.,0.,0.));
#22848=CARTESIAN_POINT('Origin',(38.7298334620742,3.5,13.));
#22849=CARTESIAN_POINT('',(38.1248334620742,5.,13.));
#22850=CARTESIAN_POINT('Origin',(38.7298334620742,5.,13.));
#22851=CARTESIAN_POINT('',(38.1248334620742,3.5,13.));
#22852=CARTESIAN_POINT('',(38.1248334620742,3.5,13.));
#22853=CARTESIAN_POINT('Origin',(38.7298334620742,3.5,13.));
#22854=CARTESIAN_POINT('Origin',(38.7298334620742,3.5,13.));
#22855=CARTESIAN_POINT('',(37.9298334620742,5.,13.));
#22856=CARTESIAN_POINT('Origin',(38.7298334620742,5.,13.));
#22857=CARTESIAN_POINT('',(37.9298334620742,3.5,13.));
#22858=CARTESIAN_POINT('',(37.9298334620742,3.5,13.));
#22859=CARTESIAN_POINT('Origin',(38.7298334620742,3.5,13.));
#22860=CARTESIAN_POINT('Origin',(38.7298334620742,5.,13.));
#22861=CARTESIAN_POINT('Origin',(38.7298334620742,3.5,13.));
#22862=CARTESIAN_POINT('',(0.,0.,0.));
#22863=CARTESIAN_POINT('Origin',(38.7298334620742,6.,13.));
#22864=CARTESIAN_POINT('',(38.1248334620742,6.5,13.));
#22865=CARTESIAN_POINT('Origin',(38.7298334620742,6.5,13.));
#22866=CARTESIAN_POINT('',(38.1248334620742,6.,13.));
#22867=CARTESIAN_POINT('',(38.1248334620742,6.,13.));
#22868=CARTESIAN_POINT('Origin',(38.7298334620742,6.,13.));
#22869=CARTESIAN_POINT('Origin',(38.7298334620742,6.,13.));
#22870=CARTESIAN_POINT('',(37.9298334620742,6.5,13.));
#22871=CARTESIAN_POINT('Origin',(38.7298334620742,6.5,13.));
#22872=CARTESIAN_POINT('',(37.9298334620742,6.,13.));
#22873=CARTESIAN_POINT('',(37.9298334620742,6.,13.));
#22874=CARTESIAN_POINT('Origin',(38.7298334620742,6.,13.));
#22875=CARTESIAN_POINT('Origin',(38.7298334620742,6.5,13.));
#22876=CARTESIAN_POINT('Origin',(38.7298334620742,6.,13.));
#22877=CARTESIAN_POINT('',(0.,0.,0.));
#22878=CARTESIAN_POINT('',(0.,0.,0.));
#22879=CARTESIAN_POINT('Origin',(0.75,1.2,0.));
#22880=CARTESIAN_POINT('',(0.885663593019381,1.2,-0.16));
#22881=CARTESIAN_POINT('',(0.885663593019381,1.2,0.16));
#22882=CARTESIAN_POINT('Origin',(0.,1.2,0.));
#22883=CARTESIAN_POINT('',(0.93,1.2,-0.16));
#22884=CARTESIAN_POINT('',(0.93,1.2,-0.16));
#22885=CARTESIAN_POINT('',(0.93,1.2,0.16));
#22886=CARTESIAN_POINT('',(0.93,1.2,0.16));
#22887=CARTESIAN_POINT('',(0.57,1.2,0.16));
#22888=CARTESIAN_POINT('Origin',(0.57,0.,0.16));
#22889=CARTESIAN_POINT('',(0.885663593019381,-1.2,0.16));
#22890=CARTESIAN_POINT('',(0.885663593019381,0.,0.16));
#22891=CARTESIAN_POINT('',(0.93,-1.2,0.16));
#22892=CARTESIAN_POINT('',(0.93,0.,0.16));
#22893=CARTESIAN_POINT('',(0.57,-1.2,0.16));
#22894=CARTESIAN_POINT('Origin',(0.75,-1.2,0.));
#22895=CARTESIAN_POINT('',(0.885663593019381,-1.2,-0.16));
#22896=CARTESIAN_POINT('Origin',(0.,-1.2,0.));
#22897=CARTESIAN_POINT('',(0.93,-1.2,-0.16));
#22898=CARTESIAN_POINT('',(0.93,-1.2,0.16));
#22899=CARTESIAN_POINT('',(0.93,-1.2,-0.16));
#22900=CARTESIAN_POINT('Origin',(0.93,0.,-0.16));
#22901=CARTESIAN_POINT('',(0.885663593019381,0.,-0.16));
#22902=CARTESIAN_POINT('',(0.93,0.,-0.16));
#22903=CARTESIAN_POINT('Origin',(0.93,0.,0.16));
#22904=CARTESIAN_POINT('Origin',(1.05,1.5,0.));
#22905=CARTESIAN_POINT('',(-1.05,1.5,-1.28587913910472E-16));
#22906=CARTESIAN_POINT('Origin',(0.,1.5,0.));
#22907=CARTESIAN_POINT('',(-0.9,1.5,-1.10218211923262E-16));
#22908=CARTESIAN_POINT('Origin',(0.,1.5,0.));
#22909=CARTESIAN_POINT('Origin',(0.,1.315,0.));
#22910=CARTESIAN_POINT('',(-1.05,1.13,-1.28587913910472E-16));
#22911=CARTESIAN_POINT('Origin',(0.,1.13,0.));
#22912=CARTESIAN_POINT('',(-1.05,1.315,-1.28587913910472E-16));
#22913=CARTESIAN_POINT('Origin',(1.,1.13,0.));
#22914=CARTESIAN_POINT('',(-1.,1.13,-1.22464679914735E-16));
#22915=CARTESIAN_POINT('Origin',(0.,1.13,0.));
#22916=CARTESIAN_POINT('Origin',(0.,1.065,0.));
#22917=CARTESIAN_POINT('',(-1.,1.,-1.22464679914735E-16));
#22918=CARTESIAN_POINT('Origin',(0.,1.,0.));
#22919=CARTESIAN_POINT('',(-1.,1.065,-1.22464679914735E-16));
#22920=CARTESIAN_POINT('Origin',(1.05,1.,0.));
#22921=CARTESIAN_POINT('',(-1.05,1.,-1.28587913910472E-16));
#22922=CARTESIAN_POINT('Origin',(0.,1.,0.));
#22923=CARTESIAN_POINT('Origin',(0.,0.,0.));
#22924=CARTESIAN_POINT('',(-1.05,-1.,-1.28587913910472E-16));
#22925=CARTESIAN_POINT('Origin',(0.,-1.,0.));
#22926=CARTESIAN_POINT('',(-1.05,0.,-1.28587913910472E-16));
#22927=CARTESIAN_POINT('Origin',(1.,-1.,0.));
#22928=CARTESIAN_POINT('',(-1.,-1.,-1.22464679914735E-16));
#22929=CARTESIAN_POINT('Origin',(0.,-1.,0.));
#22930=CARTESIAN_POINT('Origin',(0.,-1.065,0.));
#22931=CARTESIAN_POINT('',(-1.,-1.13,-1.22464679914735E-16));
#22932=CARTESIAN_POINT('Origin',(0.,-1.13,0.));
#22933=CARTESIAN_POINT('',(-1.,-1.065,-1.22464679914735E-16));
#22934=CARTESIAN_POINT('Origin',(1.05,-1.13,0.));
#22935=CARTESIAN_POINT('',(-1.05,-1.13,-1.28587913910472E-16));
#22936=CARTESIAN_POINT('Origin',(0.,-1.13,0.));
#22937=CARTESIAN_POINT('Origin',(0.,-1.315,0.));
#22938=CARTESIAN_POINT('',(-1.05,-1.5,-1.28587913910472E-16));
#22939=CARTESIAN_POINT('Origin',(0.,-1.5,0.));
#22940=CARTESIAN_POINT('',(-1.05,-1.315,-1.28587913910472E-16));
#22941=CARTESIAN_POINT('Origin',(0.9,-1.5,0.));
#22942=CARTESIAN_POINT('',(-0.9,-1.5,-1.10218211923262E-16));
#22943=CARTESIAN_POINT('Origin',(0.,-1.5,0.));
#22944=CARTESIAN_POINT('Origin',(0.,0.,0.));
#22945=CARTESIAN_POINT('',(-0.9,0.,-1.10218211923262E-16));
#22946=CARTESIAN_POINT('',(0.,0.,0.));
#22947=CARTESIAN_POINT('Origin',(0.75,1.2,0.));
#22948=CARTESIAN_POINT('',(0.880582193778639,1.2,0.16));
#22949=CARTESIAN_POINT('',(0.880582193778639,1.2,-0.16));
#22950=CARTESIAN_POINT('Origin',(0.,1.2,0.));
#22951=CARTESIAN_POINT('',(0.583459510163302,1.2,0.16));
#22952=CARTESIAN_POINT('',(0.57,1.2,0.16));
#22953=CARTESIAN_POINT('',(0.583459510163302,1.2,-0.16));
#22954=CARTESIAN_POINT('Origin',(0.,1.2,0.));
#22955=CARTESIAN_POINT('',(0.93,1.2,-0.16));
#22956=CARTESIAN_POINT('Origin',(0.93,0.,-0.16));
#22957=CARTESIAN_POINT('',(0.880582193778639,-1.2,-0.16));
#22958=CARTESIAN_POINT('',(0.880582193778639,0.,-0.16));
#22959=CARTESIAN_POINT('',(0.583459510163302,-1.2,-0.16));
#22960=CARTESIAN_POINT('',(0.583459510163302,0.,-0.16));
#22961=CARTESIAN_POINT('',(0.93,-1.2,-0.16));
#22962=CARTESIAN_POINT('Origin',(0.75,-1.2,0.));
#22963=CARTESIAN_POINT('',(0.880582193778639,-1.2,0.16));
#22964=CARTESIAN_POINT('Origin',(0.,-1.2,0.));
#22965=CARTESIAN_POINT('',(0.583459510163302,-1.2,0.16));
#22966=CARTESIAN_POINT('Origin',(0.,-1.2,0.));
#22967=CARTESIAN_POINT('',(0.57,-1.2,0.16));
#22968=CARTESIAN_POINT('Origin',(0.57,0.,0.16));
#22969=CARTESIAN_POINT('',(0.880582193778639,0.,0.16));
#22970=CARTESIAN_POINT('',(0.583459510163302,0.,0.16));
#22971=CARTESIAN_POINT('Origin',(0.895,1.35,0.));
#22972=CARTESIAN_POINT('',(-0.895,1.35,-1.09605888523688E-16));
#22973=CARTESIAN_POINT('Origin',(0.,1.35,0.));
#22974=CARTESIAN_POINT('',(-0.605,1.35,-7.40911313484149E-17));
#22975=CARTESIAN_POINT('Origin',(0.,1.35,0.));
#22976=CARTESIAN_POINT('Origin',(0.,0.,0.));
#22977=CARTESIAN_POINT('',(-0.895,-1.35,-1.09605888523688E-16));
#22978=CARTESIAN_POINT('Origin',(0.,-1.35,0.));
#22979=CARTESIAN_POINT('',(-0.895,0.,-1.09605888523688E-16));
#22980=CARTESIAN_POINT('Origin',(0.605,-1.35,0.));
#22981=CARTESIAN_POINT('',(-0.605,-1.35,-7.40911313484149E-17));
#22982=CARTESIAN_POINT('Origin',(0.,-1.35,0.));
#22983=CARTESIAN_POINT('Origin',(0.,0.,0.));
#22984=CARTESIAN_POINT('',(-0.605,0.,-7.40911313484149E-17));
#22985=CARTESIAN_POINT('',(0.,0.,0.));
#22986=CARTESIAN_POINT('',(0.,0.,0.));
#22987=CARTESIAN_POINT('',(0.,0.,0.));
#22988=CARTESIAN_POINT('Origin',(0.,-0.4,0.));
#22989=CARTESIAN_POINT('',(-0.1954,-0.4,2.39295984553393E-17));
#22990=CARTESIAN_POINT('Origin',(0.,-0.4,0.));
#22991=CARTESIAN_POINT('Origin',(0.0577350269189626,0.,-0.1));
#22992=CARTESIAN_POINT('',(0.0577350269189626,0.,-0.1));
#22993=CARTESIAN_POINT('',(0.115470053837925,0.,0.));
#22994=CARTESIAN_POINT('',(0.0934187836487032,0.,-0.0381939203391614));
#22995=CARTESIAN_POINT('',(0.0577350269189626,-0.2,-0.1));
#22996=CARTESIAN_POINT('',(0.0577350269189626,0.,-0.1));
#22997=CARTESIAN_POINT('',(0.115470053837925,-0.2,0.));
#22998=CARTESIAN_POINT('',(0.115470053837925,-0.2,0.));
#22999=CARTESIAN_POINT('',(0.115470053837925,0.,0.));
#23000=CARTESIAN_POINT('Origin',(-0.0577350269189626,0.,-0.1));
#23001=CARTESIAN_POINT('',(-0.0577350269189626,0.,-0.1));
#23002=CARTESIAN_POINT('',(0.0561324865405187,0.,-0.1));
#23003=CARTESIAN_POINT('',(-0.0577350269189626,-0.2,-0.1));
#23004=CARTESIAN_POINT('',(-0.0577350269189626,0.,-0.1));
#23005=CARTESIAN_POINT('',(0.0577350269189626,-0.2,-0.1));
#23006=CARTESIAN_POINT('Origin',(-0.115470053837925,0.,-1.38777878078145E-17));
#23007=CARTESIAN_POINT('',(-0.115470053837925,0.,-1.41410031829988E-17));
#23008=CARTESIAN_POINT('',(-0.0797862971081845,0.,-0.0618060796608387));
#23009=CARTESIAN_POINT('',(-0.115470053837925,-0.2,-1.38777878078145E-17));
#23010=CARTESIAN_POINT('',(-0.115470053837925,0.,-1.41410031829988E-17));
#23011=CARTESIAN_POINT('',(-0.0577350269189626,-0.2,-0.1));
#23012=CARTESIAN_POINT('Origin',(-0.0577350269189626,0.,0.1));
#23013=CARTESIAN_POINT('',(-0.0577350269189626,0.,0.1));
#23014=CARTESIAN_POINT('',(-0.0509187836487033,0.,0.111806079660839));
#23015=CARTESIAN_POINT('',(-0.0577350269189626,-0.2,0.1));
#23016=CARTESIAN_POINT('',(-0.0577350269189626,0.,0.1));
#23017=CARTESIAN_POINT('',(-0.115470053837925,-0.2,-1.41410031829988E-17));
#23018=CARTESIAN_POINT('Origin',(0.0577350269189626,0.,0.1));
#23019=CARTESIAN_POINT('',(0.0577350269189626,0.,0.1));
#23020=CARTESIAN_POINT('',(0.113867513459481,0.,0.1));
#23021=CARTESIAN_POINT('',(0.0577350269189626,-0.2,0.1));
#23022=CARTESIAN_POINT('',(0.0577350269189626,0.,0.1));
#23023=CARTESIAN_POINT('',(-0.0577350269189626,-0.2,0.1));
#23024=CARTESIAN_POINT('Origin',(0.115470053837925,0.,0.));
#23025=CARTESIAN_POINT('',(0.122286297108185,0.,-0.0118060796608386));
#23026=CARTESIAN_POINT('',(0.0577350269189626,-0.2,0.1));
#23027=CARTESIAN_POINT('Origin',(0.,-0.2,0.));
#23028=CARTESIAN_POINT('Origin',(0.17,0.,0.));
#23029=CARTESIAN_POINT('',(-0.17,-8.67361737988404E-18,-2.0818995585505E-17));
#23030=CARTESIAN_POINT('Origin',(0.,0.,0.));
#23031=CARTESIAN_POINT('Origin',(0.,-0.015,0.));
#23032=CARTESIAN_POINT('',(-0.1954,-0.0254,-2.39295984553393E-17));
#23033=CARTESIAN_POINT('Origin',(0.,-0.0254,0.));
#23034=CARTESIAN_POINT('',(-0.185,-0.015,-2.2655965784226E-17));
#23035=CARTESIAN_POINT('Origin',(0.,-0.2775,0.));
#23036=CARTESIAN_POINT('',(-0.1954,-0.2775,-2.39295984553393E-17));
#23037=CARTESIAN_POINT('',(0.,0.,0.));
#23038=CARTESIAN_POINT('',(0.,0.,0.));
#23039=CARTESIAN_POINT('Origin',(19.3649167310371,-7.1,8.));
#23040=CARTESIAN_POINT('',(18.3649167310371,-7.,8.));
#23041=CARTESIAN_POINT('Origin',(19.3649167310371,-7.,8.));
#23042=CARTESIAN_POINT('',(18.3649167310371,-6.,8.));
#23043=CARTESIAN_POINT('',(18.3649167310371,-7.1,8.));
#23044=CARTESIAN_POINT('Origin',(19.3649167310371,-6.,8.));
#23045=CARTESIAN_POINT('Origin',(19.3649167310371,-7.,8.));
#23046=CARTESIAN_POINT('',(18.1934954781404,-7.,8.93689500386222));
#23047=CARTESIAN_POINT('',(18.1934954781404,-6.,8.93689500386223));
#23048=CARTESIAN_POINT('',(18.1934954781404,-7.,8.93689500386223));
#23049=CARTESIAN_POINT('',(19.9363379839338,-7.,9.38689500386222));
#23050=CARTESIAN_POINT('Origin',(19.3649167310371,-7.,8.));
#23051=CARTESIAN_POINT('',(19.9363379839338,-6.,9.38689500386223));
#23052=CARTESIAN_POINT('',(19.9363379839338,-7.,9.38689500386223));
#23053=CARTESIAN_POINT('Origin',(19.3649167310371,-6.,8.));
#23054=CARTESIAN_POINT('Origin',(19.3649167310371,-7.,8.));
#23055=CARTESIAN_POINT('',(18.7934954781404,-6.,6.61310499613778));
#23056=CARTESIAN_POINT('',(18.7934954781404,-7.,6.61310499613778));
#23057=CARTESIAN_POINT('',(18.7934954781404,-7.,6.61310499613778));
#23058=CARTESIAN_POINT('',(20.5363379839338,-6.,7.06310499613778));
#23059=CARTESIAN_POINT('Origin',(19.3649167310371,-6.,8.));
#23060=CARTESIAN_POINT('',(20.5363379839338,-7.,7.06310499613778));
#23061=CARTESIAN_POINT('',(20.5363379839338,-7.,7.06310499613778));
#23062=CARTESIAN_POINT('Origin',(19.3649167310371,-7.,8.));
#23063=CARTESIAN_POINT('Origin',(39.0298334620742,-7.,11.8381049961378));
#23064=CARTESIAN_POINT('',(38.1584122091775,-6.,11.6131049961378));
#23065=CARTESIAN_POINT('',(39.0298334620742,-6.,11.8381049961378));
#23066=CARTESIAN_POINT('',(38.1584122091775,-7.,11.6131049961378));
#23067=CARTESIAN_POINT('',(38.1584122091775,-7.,11.6131049961378));
#23068=CARTESIAN_POINT('',(39.0298334620742,-7.,11.8381049961378));
#23069=CARTESIAN_POINT('Origin',(39.0298334620742,-7.,11.8381049961378));
#23070=CARTESIAN_POINT('',(1.17142125289667,-7.,2.06310499613778));
#23071=CARTESIAN_POINT('',(39.0298334620742,-7.,11.8381049961378));
#23072=CARTESIAN_POINT('',(1.17142125289667,-6.,2.06310499613778));
#23073=CARTESIAN_POINT('',(1.17142125289667,-7.,2.06310499613778));
#23074=CARTESIAN_POINT('',(39.0298334620742,-6.,11.8381049961378));
#23075=CARTESIAN_POINT('Origin',(-0.3,-7.,4.16189500386223));
#23076=CARTESIAN_POINT('',(37.5584122091775,-7.,13.9368950038622));
#23077=CARTESIAN_POINT('',(-0.3,-7.,4.16189500386223));
#23078=CARTESIAN_POINT('',(37.5584122091775,-6.,13.9368950038622));
#23079=CARTESIAN_POINT('',(37.5584122091775,-7.,13.9368950038622));
#23080=CARTESIAN_POINT('',(-0.3,-6.,4.16189500386223));
#23081=CARTESIAN_POINT('Origin',(38.7298334620742,-7.1,13.));
#23082=CARTESIAN_POINT('',(37.7298334620742,-7.,13.));
#23083=CARTESIAN_POINT('Origin',(38.7298334620742,-7.,13.));
#23084=CARTESIAN_POINT('',(37.7298334620742,-6.,13.));
#23085=CARTESIAN_POINT('',(37.7298334620742,-7.1,13.));
#23086=CARTESIAN_POINT('Origin',(38.7298334620742,-6.,13.));
#23087=CARTESIAN_POINT('Origin',(38.7298334620742,-7.,13.));
#23088=CARTESIAN_POINT('Origin',(38.7298334620742,-6.,13.));
#23089=CARTESIAN_POINT('Origin',(38.7298334620742,-7.,13.));
#23090=CARTESIAN_POINT('Origin',(19.3649167310371,-7.,8.));
#23091=CARTESIAN_POINT('',(0.571421252896668,-7.,4.38689500386223));
#23092=CARTESIAN_POINT('',(-0.3,-7.,4.16189500386223));
#23093=CARTESIAN_POINT('Origin',(0.,-7.,3.));
#23094=CARTESIAN_POINT('',(-1.,-7.,3.));
#23095=CARTESIAN_POINT('Origin',(0.,-7.,3.));
#23096=CARTESIAN_POINT('Origin',(-0.3,-7.,4.16189500386223));
#23097=CARTESIAN_POINT('',(0.571421252896668,-6.,4.38689500386223));
#23098=CARTESIAN_POINT('',(-0.3,-6.,4.16189500386223));
#23099=CARTESIAN_POINT('',(0.571421252896668,-7.,4.38689500386223));
#23100=CARTESIAN_POINT('Origin',(0.,-7.1,3.));
#23101=CARTESIAN_POINT('',(-1.,-6.,3.));
#23102=CARTESIAN_POINT('',(-1.,-7.1,3.));
#23103=CARTESIAN_POINT('Origin',(0.,-6.,3.));
#23104=CARTESIAN_POINT('Origin',(0.,-7.,3.));
#23105=CARTESIAN_POINT('Origin',(0.,-6.,3.));
#23106=CARTESIAN_POINT('Origin',(19.3649167310371,-6.,8.));
#23107=CARTESIAN_POINT('',(0.,0.,0.));
#23108=CARTESIAN_POINT('Origin',(0.,-7.,3.));
#23109=CARTESIAN_POINT('',(-0.605,-6.,3.));
#23110=CARTESIAN_POINT('Origin',(0.,-6.,3.));
#23111=CARTESIAN_POINT('',(-0.605,-7.,3.));
#23112=CARTESIAN_POINT('',(-0.605,-7.,3.));
#23113=CARTESIAN_POINT('Origin',(0.,-7.,3.));
#23114=CARTESIAN_POINT('Origin',(0.,-7.,3.));
#23115=CARTESIAN_POINT('',(-1.,-6.,3.));
#23116=CARTESIAN_POINT('Origin',(0.,-6.,3.));
#23117=CARTESIAN_POINT('',(-1.,-7.,3.));
#23118=CARTESIAN_POINT('',(-1.,-7.,3.));
#23119=CARTESIAN_POINT('Origin',(0.,-7.,3.));
#23120=CARTESIAN_POINT('Origin',(0.,-6.,3.));
#23121=CARTESIAN_POINT('Origin',(0.,-7.,3.));
#23122=CARTESIAN_POINT('',(0.,0.,0.));
#23123=CARTESIAN_POINT('Origin',(38.7298334620742,-7.,13.));
#23124=CARTESIAN_POINT('',(38.1248334620742,-6.,13.));
#23125=CARTESIAN_POINT('Origin',(38.7298334620742,-6.,13.));
#23126=CARTESIAN_POINT('',(38.1248334620742,-7.,13.));
#23127=CARTESIAN_POINT('',(38.1248334620742,-7.,13.));
#23128=CARTESIAN_POINT('Origin',(38.7298334620742,-7.,13.));
#23129=CARTESIAN_POINT('Origin',(38.7298334620742,-7.,13.));
#23130=CARTESIAN_POINT('',(37.7298334620742,-6.,13.));
#23131=CARTESIAN_POINT('Origin',(38.7298334620742,-6.,13.));
#23132=CARTESIAN_POINT('',(37.7298334620742,-7.,13.));
#23133=CARTESIAN_POINT('',(37.7298334620742,-7.,13.));
#23134=CARTESIAN_POINT('Origin',(38.7298334620742,-7.,13.));
#23135=CARTESIAN_POINT('Origin',(38.7298334620742,-6.,13.));
#23136=CARTESIAN_POINT('Origin',(38.7298334620742,-7.,13.));
#23137=CARTESIAN_POINT('',(0.,0.,0.));
#23138=CARTESIAN_POINT('Origin',(19.3649167310371,-7.,8.));
#23139=CARTESIAN_POINT('',(18.7599167310371,-6.,8.));
#23140=CARTESIAN_POINT('Origin',(19.3649167310371,-6.,8.));
#23141=CARTESIAN_POINT('',(18.7599167310371,-7.,8.));
#23142=CARTESIAN_POINT('',(18.7599167310371,-7.,8.));
#23143=CARTESIAN_POINT('Origin',(19.3649167310371,-7.,8.));
#23144=CARTESIAN_POINT('Origin',(19.3649167310371,-7.,8.));
#23145=CARTESIAN_POINT('',(18.3649167310371,-6.,8.));
#23146=CARTESIAN_POINT('Origin',(19.3649167310371,-6.,8.));
#23147=CARTESIAN_POINT('',(18.3649167310371,-7.,8.));
#23148=CARTESIAN_POINT('',(18.3649167310371,-7.,8.));
#23149=CARTESIAN_POINT('Origin',(19.3649167310371,-7.,8.));
#23150=CARTESIAN_POINT('Origin',(19.3649167310371,-6.,8.));
#23151=CARTESIAN_POINT('Origin',(19.3649167310371,-7.,8.));
#23152=CARTESIAN_POINT('',(0.,0.,0.));
#23153=CARTESIAN_POINT('Origin',(19.3649167310371,4.9,8.));
#23154=CARTESIAN_POINT('',(18.3649167310371,5.,8.));
#23155=CARTESIAN_POINT('Origin',(19.3649167310371,5.,8.));
#23156=CARTESIAN_POINT('',(18.3649167310371,6.,8.));
#23157=CARTESIAN_POINT('',(18.3649167310371,4.9,8.));
#23158=CARTESIAN_POINT('Origin',(19.3649167310371,6.,8.));
#23159=CARTESIAN_POINT('Origin',(19.3649167310371,5.,8.));
#23160=CARTESIAN_POINT('',(18.1934954781404,5.,8.93689500386222));
#23161=CARTESIAN_POINT('',(18.1934954781404,6.,8.93689500386223));
#23162=CARTESIAN_POINT('',(18.1934954781404,5.,8.93689500386223));
#23163=CARTESIAN_POINT('',(19.9363379839338,5.,9.38689500386222));
#23164=CARTESIAN_POINT('Origin',(19.3649167310371,5.,8.));
#23165=CARTESIAN_POINT('',(19.9363379839338,6.,9.38689500386223));
#23166=CARTESIAN_POINT('',(19.9363379839338,5.,9.38689500386223));
#23167=CARTESIAN_POINT('Origin',(19.3649167310371,6.,8.));
#23168=CARTESIAN_POINT('Origin',(19.3649167310371,5.,8.));
#23169=CARTESIAN_POINT('',(18.7934954781404,6.,6.61310499613778));
#23170=CARTESIAN_POINT('',(18.7934954781404,5.,6.61310499613778));
#23171=CARTESIAN_POINT('',(18.7934954781404,5.,6.61310499613778));
#23172=CARTESIAN_POINT('',(20.5363379839338,6.,7.06310499613778));
#23173=CARTESIAN_POINT('Origin',(19.3649167310371,6.,8.));
#23174=CARTESIAN_POINT('',(20.5363379839338,5.,7.06310499613778));
#23175=CARTESIAN_POINT('',(20.5363379839338,5.,7.06310499613778));
#23176=CARTESIAN_POINT('Origin',(19.3649167310371,5.,8.));
#23177=CARTESIAN_POINT('Origin',(39.0298334620742,5.,11.8381049961378));
#23178=CARTESIAN_POINT('',(38.1584122091775,6.,11.6131049961378));
#23179=CARTESIAN_POINT('',(39.0298334620742,6.,11.8381049961378));
#23180=CARTESIAN_POINT('',(38.1584122091775,5.,11.6131049961378));
#23181=CARTESIAN_POINT('',(38.1584122091775,5.,11.6131049961378));
#23182=CARTESIAN_POINT('',(39.0298334620742,5.,11.8381049961378));
#23183=CARTESIAN_POINT('Origin',(39.0298334620742,5.,11.8381049961378));
#23184=CARTESIAN_POINT('',(1.17142125289667,5.,2.06310499613778));
#23185=CARTESIAN_POINT('',(39.0298334620742,5.,11.8381049961378));
#23186=CARTESIAN_POINT('',(1.17142125289667,6.,2.06310499613778));
#23187=CARTESIAN_POINT('',(1.17142125289667,5.,2.06310499613778));
#23188=CARTESIAN_POINT('',(39.0298334620742,6.,11.8381049961378));
#23189=CARTESIAN_POINT('Origin',(-0.3,5.,4.16189500386223));
#23190=CARTESIAN_POINT('',(37.5584122091775,5.,13.9368950038622));
#23191=CARTESIAN_POINT('',(-0.3,5.,4.16189500386223));
#23192=CARTESIAN_POINT('',(37.5584122091775,6.,13.9368950038622));
#23193=CARTESIAN_POINT('',(37.5584122091775,5.,13.9368950038622));
#23194=CARTESIAN_POINT('',(-0.3,6.,4.16189500386223));
#23195=CARTESIAN_POINT('Origin',(38.7298334620742,4.9,13.));
#23196=CARTESIAN_POINT('',(37.7298334620742,5.,13.));
#23197=CARTESIAN_POINT('Origin',(38.7298334620742,5.,13.));
#23198=CARTESIAN_POINT('',(37.7298334620742,6.,13.));
#23199=CARTESIAN_POINT('',(37.7298334620742,4.9,13.));
#23200=CARTESIAN_POINT('Origin',(38.7298334620742,6.,13.));
#23201=CARTESIAN_POINT('Origin',(38.7298334620742,5.,13.));
#23202=CARTESIAN_POINT('Origin',(38.7298334620742,6.,13.));
#23203=CARTESIAN_POINT('Origin',(38.7298334620742,5.,13.));
#23204=CARTESIAN_POINT('Origin',(19.3649167310371,5.,8.));
#23205=CARTESIAN_POINT('',(0.571421252896668,5.,4.38689500386223));
#23206=CARTESIAN_POINT('',(-0.3,5.,4.16189500386223));
#23207=CARTESIAN_POINT('Origin',(0.,5.,3.));
#23208=CARTESIAN_POINT('',(-1.,5.,3.));
#23209=CARTESIAN_POINT('Origin',(0.,5.,3.));
#23210=CARTESIAN_POINT('Origin',(-0.3,5.,4.16189500386223));
#23211=CARTESIAN_POINT('',(0.571421252896668,6.,4.38689500386223));
#23212=CARTESIAN_POINT('',(-0.3,6.,4.16189500386223));
#23213=CARTESIAN_POINT('',(0.571421252896668,5.,4.38689500386223));
#23214=CARTESIAN_POINT('Origin',(0.,4.9,3.));
#23215=CARTESIAN_POINT('',(-1.,6.,3.));
#23216=CARTESIAN_POINT('',(-1.,4.9,3.));
#23217=CARTESIAN_POINT('Origin',(0.,6.,3.));
#23218=CARTESIAN_POINT('Origin',(0.,5.,3.));
#23219=CARTESIAN_POINT('Origin',(0.,6.,3.));
#23220=CARTESIAN_POINT('Origin',(19.3649167310371,6.,8.));
#23221=CARTESIAN_POINT('',(0.,0.,0.));
#23222=CARTESIAN_POINT('Origin',(0.,5.,3.));
#23223=CARTESIAN_POINT('',(-0.605,6.,3.));
#23224=CARTESIAN_POINT('Origin',(0.,6.,3.));
#23225=CARTESIAN_POINT('',(-0.605,5.,3.));
#23226=CARTESIAN_POINT('',(-0.605,5.,3.));
#23227=CARTESIAN_POINT('Origin',(0.,5.,3.));
#23228=CARTESIAN_POINT('Origin',(0.,5.,3.));
#23229=CARTESIAN_POINT('',(-1.,6.,3.));
#23230=CARTESIAN_POINT('Origin',(0.,6.,3.));
#23231=CARTESIAN_POINT('',(-1.,5.,3.));
#23232=CARTESIAN_POINT('',(-1.,5.,3.));
#23233=CARTESIAN_POINT('Origin',(0.,5.,3.));
#23234=CARTESIAN_POINT('Origin',(0.,6.,3.));
#23235=CARTESIAN_POINT('Origin',(0.,5.,3.));
#23236=CARTESIAN_POINT('',(0.,0.,0.));
#23237=CARTESIAN_POINT('Origin',(38.7298334620742,5.,13.));
#23238=CARTESIAN_POINT('',(38.1248334620742,6.,13.));
#23239=CARTESIAN_POINT('Origin',(38.7298334620742,6.,13.));
#23240=CARTESIAN_POINT('',(38.1248334620742,5.,13.));
#23241=CARTESIAN_POINT('',(38.1248334620742,5.,13.));
#23242=CARTESIAN_POINT('Origin',(38.7298334620742,5.,13.));
#23243=CARTESIAN_POINT('Origin',(38.7298334620742,5.,13.));
#23244=CARTESIAN_POINT('',(37.7298334620742,6.,13.));
#23245=CARTESIAN_POINT('Origin',(38.7298334620742,6.,13.));
#23246=CARTESIAN_POINT('',(37.7298334620742,5.,13.));
#23247=CARTESIAN_POINT('',(37.7298334620742,5.,13.));
#23248=CARTESIAN_POINT('Origin',(38.7298334620742,5.,13.));
#23249=CARTESIAN_POINT('Origin',(38.7298334620742,6.,13.));
#23250=CARTESIAN_POINT('Origin',(38.7298334620742,5.,13.));
#23251=CARTESIAN_POINT('',(0.,0.,0.));
#23252=CARTESIAN_POINT('Origin',(19.3649167310371,5.,8.));
#23253=CARTESIAN_POINT('',(18.7599167310371,6.,8.));
#23254=CARTESIAN_POINT('Origin',(19.3649167310371,6.,8.));
#23255=CARTESIAN_POINT('',(18.7599167310371,5.,8.));
#23256=CARTESIAN_POINT('',(18.7599167310371,5.,8.));
#23257=CARTESIAN_POINT('Origin',(19.3649167310371,5.,8.));
#23258=CARTESIAN_POINT('Origin',(19.3649167310371,5.,8.));
#23259=CARTESIAN_POINT('',(18.3649167310371,6.,8.));
#23260=CARTESIAN_POINT('Origin',(19.3649167310371,6.,8.));
#23261=CARTESIAN_POINT('',(18.3649167310371,5.,8.));
#23262=CARTESIAN_POINT('',(18.3649167310371,5.,8.));
#23263=CARTESIAN_POINT('Origin',(19.3649167310371,5.,8.));
#23264=CARTESIAN_POINT('Origin',(19.3649167310371,6.,8.));
#23265=CARTESIAN_POINT('Origin',(19.3649167310371,5.,8.));
#23266=CARTESIAN_POINT('',(0.,0.,0.));
#23267=CARTESIAN_POINT('Origin',(19.3649167310371,6.9,8.));
#23268=CARTESIAN_POINT('',(19.1999167310371,6.9,8.));
#23269=CARTESIAN_POINT('Origin',(19.3649167310371,6.9,8.));
#23270=CARTESIAN_POINT('',(19.1999167310371,8.5,8.));
#23271=CARTESIAN_POINT('',(19.1999167310371,6.9,8.));
#23272=CARTESIAN_POINT('Origin',(19.3649167310371,8.5,8.));
#23273=CARTESIAN_POINT('Origin',(19.3649167310371,6.9,8.));
#23274=CARTESIAN_POINT('Origin',(19.3649167310371,-7.6,8.));
#23275=CARTESIAN_POINT('',(19.1999167310371,-7.5,8.));
#23276=CARTESIAN_POINT('Origin',(19.3649167310371,-7.5,8.));
#23277=CARTESIAN_POINT('',(19.1999167310371,-5.9,8.));
#23278=CARTESIAN_POINT('',(19.1999167310371,-7.6,8.));
#23279=CARTESIAN_POINT('Origin',(19.3649167310371,-5.9,8.));
#23280=CARTESIAN_POINT('Origin',(19.3649167310371,-5.9,8.));
#23281=CARTESIAN_POINT('Origin',(19.3649167310371,-7.5,8.));
#23282=CARTESIAN_POINT('',(18.7649167310371,8.5,8.));
#23283=CARTESIAN_POINT('Origin',(19.3649167310371,8.5,8.));
#23284=CARTESIAN_POINT('',(18.7649167310371,-7.5,8.));
#23285=CARTESIAN_POINT('',(18.7649167310371,-7.5,8.));
#23286=CARTESIAN_POINT('Origin',(19.3649167310371,-7.5,8.));
#23287=CARTESIAN_POINT('Origin',(19.3649167310371,8.5,8.));
#23288=CARTESIAN_POINT('Origin',(19.3649167310371,-7.5,8.));
#23289=CARTESIAN_POINT('',(0.,0.,0.));
#23290=CARTESIAN_POINT('Origin',(19.3649167310371,-7.7,8.));
#23291=CARTESIAN_POINT('',(19.1399167310371,-7.5,8.));
#23292=CARTESIAN_POINT('Origin',(19.3649167310371,-7.5,8.));
#23293=CARTESIAN_POINT('',(19.1399167310371,-7.7,8.));
#23294=CARTESIAN_POINT('',(19.1399167310371,-7.7,8.));
#23295=CARTESIAN_POINT('Origin',(19.3649167310371,-7.7,8.));
#23296=CARTESIAN_POINT('Origin',(19.3649167310371,-7.7,8.));
#23297=CARTESIAN_POINT('',(18.3649167310371,-7.5,8.));
#23298=CARTESIAN_POINT('Origin',(19.3649167310371,-7.5,8.));
#23299=CARTESIAN_POINT('',(18.3649167310371,-7.7,8.));
#23300=CARTESIAN_POINT('',(18.3649167310371,-7.7,8.));
#23301=CARTESIAN_POINT('Origin',(19.3649167310371,-7.7,8.));
#23302=CARTESIAN_POINT('Origin',(19.3649167310371,-7.5,8.));
#23303=CARTESIAN_POINT('Origin',(19.3649167310371,-7.7,8.));
#23304=CARTESIAN_POINT('',(0.,0.,0.));
#23305=CARTESIAN_POINT('Origin',(19.3649167310371,8.5,8.));
#23306=CARTESIAN_POINT('',(19.1399167310371,8.7,8.));
#23307=CARTESIAN_POINT('Origin',(19.3649167310371,8.7,8.));
#23308=CARTESIAN_POINT('',(19.1399167310371,8.5,8.));
#23309=CARTESIAN_POINT('',(19.1399167310371,8.5,8.));
#23310=CARTESIAN_POINT('Origin',(19.3649167310371,8.5,8.));
#23311=CARTESIAN_POINT('Origin',(19.3649167310371,8.5,8.));
#23312=CARTESIAN_POINT('',(18.3649167310371,8.7,8.));
#23313=CARTESIAN_POINT('Origin',(19.3649167310371,8.7,8.));
#23314=CARTESIAN_POINT('',(18.3649167310371,8.5,8.));
#23315=CARTESIAN_POINT('',(18.3649167310371,8.5,8.));
#23316=CARTESIAN_POINT('Origin',(19.3649167310371,8.5,8.));
#23317=CARTESIAN_POINT('Origin',(19.3649167310371,8.7,8.));
#23318=CARTESIAN_POINT('Origin',(19.3649167310371,8.5,8.));
#23319=CARTESIAN_POINT('',(0.,0.,0.));
#23320=CARTESIAN_POINT('Origin',(19.3649167310371,-7.5,8.));
#23321=CARTESIAN_POINT('',(18.7599167310371,-7.,8.));
#23322=CARTESIAN_POINT('Origin',(19.3649167310371,-7.,8.));
#23323=CARTESIAN_POINT('',(18.7599167310371,-7.5,8.));
#23324=CARTESIAN_POINT('',(18.7599167310371,-7.5,8.));
#23325=CARTESIAN_POINT('Origin',(19.3649167310371,-7.5,8.));
#23326=CARTESIAN_POINT('Origin',(19.3649167310371,-7.5,8.));
#23327=CARTESIAN_POINT('',(18.5649167310371,-7.,8.));
#23328=CARTESIAN_POINT('Origin',(19.3649167310371,-7.,8.));
#23329=CARTESIAN_POINT('',(18.5649167310371,-7.5,8.));
#23330=CARTESIAN_POINT('',(18.5649167310371,-7.5,8.));
#23331=CARTESIAN_POINT('Origin',(19.3649167310371,-7.5,8.));
#23332=CARTESIAN_POINT('Origin',(19.3649167310371,-7.,8.));
#23333=CARTESIAN_POINT('Origin',(19.3649167310371,-7.5,8.));
#23334=CARTESIAN_POINT('',(0.,0.,0.));
#23335=CARTESIAN_POINT('Origin',(19.3649167310371,-6.,8.));
#23336=CARTESIAN_POINT('',(18.7599167310371,-5.5,8.));
#23337=CARTESIAN_POINT('Origin',(19.3649167310371,-5.5,8.));
#23338=CARTESIAN_POINT('',(18.7599167310371,-6.,8.));
#23339=CARTESIAN_POINT('',(18.7599167310371,-6.,8.));
#23340=CARTESIAN_POINT('Origin',(19.3649167310371,-6.,8.));
#23341=CARTESIAN_POINT('Origin',(19.3649167310371,-6.,8.));
#23342=CARTESIAN_POINT('',(18.5649167310371,-5.5,8.));
#23343=CARTESIAN_POINT('Origin',(19.3649167310371,-5.5,8.));
#23344=CARTESIAN_POINT('',(18.5649167310371,-6.,8.));
#23345=CARTESIAN_POINT('',(18.5649167310371,-6.,8.));
#23346=CARTESIAN_POINT('Origin',(19.3649167310371,-6.,8.));
#23347=CARTESIAN_POINT('Origin',(19.3649167310371,-5.5,8.));
#23348=CARTESIAN_POINT('Origin',(19.3649167310371,-6.,8.));
#23349=CARTESIAN_POINT('',(0.,0.,0.));
#23350=CARTESIAN_POINT('Origin',(19.3649167310371,-4.5,8.));
#23351=CARTESIAN_POINT('',(18.7599167310371,5.,8.));
#23352=CARTESIAN_POINT('Origin',(19.3649167310371,5.,8.));
#23353=CARTESIAN_POINT('',(18.7599167310371,-4.5,8.));
#23354=CARTESIAN_POINT('',(18.7599167310371,-4.5,8.));
#23355=CARTESIAN_POINT('Origin',(19.3649167310371,-4.5,8.));
#23356=CARTESIAN_POINT('Origin',(19.3649167310371,-4.5,8.));
#23357=CARTESIAN_POINT('',(18.5649167310371,5.,8.));
#23358=CARTESIAN_POINT('Origin',(19.3649167310371,5.,8.));
#23359=CARTESIAN_POINT('',(18.5649167310371,-4.5,8.));
#23360=CARTESIAN_POINT('',(18.5649167310371,-4.5,8.));
#23361=CARTESIAN_POINT('Origin',(19.3649167310371,-4.5,8.));
#23362=CARTESIAN_POINT('Origin',(19.3649167310371,5.,8.));
#23363=CARTESIAN_POINT('Origin',(19.3649167310371,-4.5,8.));
#23364=CARTESIAN_POINT('',(0.,0.,0.));
#23365=CARTESIAN_POINT('Origin',(19.3649167310371,6.,8.));
#23366=CARTESIAN_POINT('',(18.7599167310371,7.,8.));
#23367=CARTESIAN_POINT('Origin',(19.3649167310371,7.,8.));
#23368=CARTESIAN_POINT('',(18.7599167310371,6.,8.));
#23369=CARTESIAN_POINT('',(18.7599167310371,6.,8.));
#23370=CARTESIAN_POINT('Origin',(19.3649167310371,6.,8.));
#23371=CARTESIAN_POINT('Origin',(19.3649167310371,6.,8.));
#23372=CARTESIAN_POINT('',(18.5649167310371,7.,8.));
#23373=CARTESIAN_POINT('Origin',(19.3649167310371,7.,8.));
#23374=CARTESIAN_POINT('',(18.5649167310371,6.,8.));
#23375=CARTESIAN_POINT('',(18.5649167310371,6.,8.));
#23376=CARTESIAN_POINT('Origin',(19.3649167310371,6.,8.));
#23377=CARTESIAN_POINT('Origin',(19.3649167310371,7.,8.));
#23378=CARTESIAN_POINT('Origin',(19.3649167310371,6.,8.));
#23379=CARTESIAN_POINT('',(0.,0.,0.));
#23380=CARTESIAN_POINT('Origin',(19.3649167310371,8.,8.));
#23381=CARTESIAN_POINT('',(18.7599167310371,8.5,8.));
#23382=CARTESIAN_POINT('Origin',(19.3649167310371,8.5,8.));
#23383=CARTESIAN_POINT('',(18.7599167310371,8.,8.));
#23384=CARTESIAN_POINT('',(18.7599167310371,8.,8.));
#23385=CARTESIAN_POINT('Origin',(19.3649167310371,8.,8.));
#23386=CARTESIAN_POINT('Origin',(19.3649167310371,8.,8.));
#23387=CARTESIAN_POINT('',(18.5649167310371,8.5,8.));
#23388=CARTESIAN_POINT('Origin',(19.3649167310371,8.5,8.));
#23389=CARTESIAN_POINT('',(18.5649167310371,8.,8.));
#23390=CARTESIAN_POINT('',(18.5649167310371,8.,8.));
#23391=CARTESIAN_POINT('Origin',(19.3649167310371,8.,8.));
#23392=CARTESIAN_POINT('Origin',(19.3649167310371,8.5,8.));
#23393=CARTESIAN_POINT('Origin',(19.3649167310371,8.,8.));
#23394=CARTESIAN_POINT('',(0.,0.,0.));
#23395=CARTESIAN_POINT('Origin',(0.3,0.4,0.));
#23396=CARTESIAN_POINT('',(-0.3,0.4,-3.67394039744206E-17));
#23397=CARTESIAN_POINT('Origin',(0.,0.4,0.));
#23398=CARTESIAN_POINT('Origin',(0.,0.375,0.));
#23399=CARTESIAN_POINT('',(-0.35,0.35,-4.28626379701573E-17));
#23400=CARTESIAN_POINT('Origin',(0.,0.35,0.));
#23401=CARTESIAN_POINT('',(-0.325,0.375,-3.9801020972289E-17));
#23402=CARTESIAN_POINT('Origin',(0.,0.19,0.));
#23403=CARTESIAN_POINT('',(-0.35,0.03,-4.28626379701574E-17));
#23404=CARTESIAN_POINT('Origin',(0.,0.03,0.));
#23405=CARTESIAN_POINT('',(-0.35,0.19,-4.28626379701574E-17));
#23406=CARTESIAN_POINT('Origin',(0.,0.0149999999999999,0.));
#23407=CARTESIAN_POINT('',(-0.32,-3.29597460435593E-17,-3.91886975727153E-17));
#23408=CARTESIAN_POINT('Origin',(0.,0.,0.));
#23409=CARTESIAN_POINT('',(-0.335,0.0149999999999999,-4.10256677714363E-17));
#23410=CARTESIAN_POINT('Origin',(0.22,0.,0.));
#23411=CARTESIAN_POINT('',(-0.22,-6.93889390390723E-18,-2.69422295812418E-17));
#23412=CARTESIAN_POINT('Origin',(0.,0.,0.));
#23413=CARTESIAN_POINT('Origin',(0.,-0.02,0.));
#23414=CARTESIAN_POINT('',(-0.1954,-0.0492,2.39295984553393E-17));
#23415=CARTESIAN_POINT('Origin',(0.,-0.0492,0.));
#23416=CARTESIAN_POINT('',(-0.21,-0.02,-2.57175827820944E-17));
#23417=CARTESIAN_POINT('Origin',(0.,-0.8,0.));
#23418=CARTESIAN_POINT('',(-0.1954,-1.5646,2.39295984553393E-17));
#23419=CARTESIAN_POINT('Origin',(0.,-1.5646,0.));
#23420=CARTESIAN_POINT('',(-0.1954,-0.8,-2.39295984553393E-17));
#23421=CARTESIAN_POINT('Origin',(0.,-1.58,0.));
#23422=CARTESIAN_POINT('',(-0.16,-1.6,-1.95943487863577E-17));
#23423=CARTESIAN_POINT('Origin',(0.,-1.6,0.));
#23424=CARTESIAN_POINT('',(-0.18,-1.58,-2.20436423846524E-17));
#23425=CARTESIAN_POINT('Origin',(0.,-1.6,0.));
#23426=CARTESIAN_POINT('Origin',(0.0866025403784439,-0.4,-0.15));
#23427=CARTESIAN_POINT('',(0.173205080756888,-0.4,0.));
#23428=CARTESIAN_POINT('',(0.0866025403784439,-0.4,-0.15));
#23429=CARTESIAN_POINT('',(0.173205080756888,-0.4,0.));
#23430=CARTESIAN_POINT('',(0.0866025403784439,-0.64,-0.15));
#23431=CARTESIAN_POINT('',(0.0866025403784439,-0.4,-0.15));
#23432=CARTESIAN_POINT('',(0.173205080756888,-0.64,0.));
#23433=CARTESIAN_POINT('',(0.173205080756888,-0.64,0.));
#23434=CARTESIAN_POINT('',(0.173205080756888,-0.4,0.));
#23435=CARTESIAN_POINT('Origin',(-0.0866025403784438,-0.4,-0.15));
#23436=CARTESIAN_POINT('',(-0.0866025403784438,-0.4,-0.15));
#23437=CARTESIAN_POINT('',(0.0866025403784439,-0.4,-0.15));
#23438=CARTESIAN_POINT('',(-0.0866025403784438,-0.64,-0.15));
#23439=CARTESIAN_POINT('',(-0.0866025403784438,-0.4,-0.15));
#23440=CARTESIAN_POINT('',(0.0866025403784439,-0.64,-0.15));
#23441=CARTESIAN_POINT('Origin',(-0.173205080756888,-0.4,-2.77555756156289E-17));
#23442=CARTESIAN_POINT('',(-0.173205080756888,-0.4,-2.12115047744981E-17));
#23443=CARTESIAN_POINT('',(-0.0866025403784438,-0.4,-0.15));
#23444=CARTESIAN_POINT('',(-0.173205080756888,-0.64,-2.77555756156289E-17));
#23445=CARTESIAN_POINT('',(-0.173205080756888,-0.4,-2.12115047744981E-17));
#23446=CARTESIAN_POINT('',(-0.0866025403784438,-0.64,-0.15));
#23447=CARTESIAN_POINT('Origin',(-0.0866025403784439,-0.4,0.15));
#23448=CARTESIAN_POINT('',(-0.0866025403784439,-0.4,0.15));
#23449=CARTESIAN_POINT('',(-0.173205080756888,-0.4,-2.12115047744981E-17));
#23450=CARTESIAN_POINT('',(-0.0866025403784439,-0.64,0.15));
#23451=CARTESIAN_POINT('',(-0.0866025403784439,-0.4,0.15));
#23452=CARTESIAN_POINT('',(-0.173205080756888,-0.64,-2.12115047744981E-17));
#23453=CARTESIAN_POINT('Origin',(0.0866025403784439,-0.4,0.15));
#23454=CARTESIAN_POINT('',(0.0866025403784439,-0.4,0.15));
#23455=CARTESIAN_POINT('',(-0.0866025403784439,-0.4,0.15));
#23456=CARTESIAN_POINT('',(0.0866025403784439,-0.64,0.15));
#23457=CARTESIAN_POINT('',(0.0866025403784439,-0.4,0.15));
#23458=CARTESIAN_POINT('',(-0.0866025403784439,-0.64,0.15));
#23459=CARTESIAN_POINT('Origin',(0.173205080756888,-0.4,0.));
#23460=CARTESIAN_POINT('',(0.0866025403784439,-0.4,0.15));
#23461=CARTESIAN_POINT('',(0.0866025403784439,-0.64,0.15));
#23462=CARTESIAN_POINT('Origin',(0.,-0.4,-2.77555756156289E-17));
#23463=CARTESIAN_POINT('Origin',(0.,-0.64,-2.77555756156289E-17));
#23464=CARTESIAN_POINT('',(0.,0.,0.));
#23465=CARTESIAN_POINT('',(0.,0.,0.));
#23466=CARTESIAN_POINT('',(0.,0.,0.));
#23467=CARTESIAN_POINT('',(0.,0.,0.));
#23468=CARTESIAN_POINT('',(0.,0.,0.));
#23469=CARTESIAN_POINT('',(0.,0.,0.));
#23470=CARTESIAN_POINT('',(0.,0.,0.));
#23471=CARTESIAN_POINT('',(0.,0.,0.));
#23472=CARTESIAN_POINT('',(0.,0.,0.));
#23473=CARTESIAN_POINT('',(0.,0.,0.));
#23474=CARTESIAN_POINT('',(0.,0.,0.));
#23475=CARTESIAN_POINT('',(0.,0.,0.));
#23476=CARTESIAN_POINT('',(-1.5,-4.,19.));
#23477=CARTESIAN_POINT('',(-1.5,4.,19.));
#23478=CARTESIAN_POINT('',(1.5,-4.,19.));
#23479=CARTESIAN_POINT('',(1.5,4.,19.));
#23480=CARTESIAN_POINT('',(43.5,-4.,19.));
#23481=CARTESIAN_POINT('',(43.5,4.,19.));
#23482=CARTESIAN_POINT('',(46.5,-4.,19.));
#23483=CARTESIAN_POINT('',(46.5,4.,19.));
#23484=CARTESIAN_POINT('',(4.93038065763132E-32,-6.2,13.));
#23485=CARTESIAN_POINT('',(0.,8.7,13.));
#23486=CARTESIAN_POINT('',(0.,0.,0.));
#23487=CARTESIAN_POINT('',(0.,0.,0.));
#23488=CARTESIAN_POINT('',(0.,0.,0.));
#23489=CARTESIAN_POINT('',(0.,0.,0.));
#23490=CARTESIAN_POINT('',(0.,0.,0.));
#23491=CARTESIAN_POINT('',(0.,0.,0.));
#23492=CARTESIAN_POINT('',(0.,0.,0.));
#23493=CARTESIAN_POINT('',(0.,0.,0.));
#23494=CARTESIAN_POINT('',(0.,0.,0.));
#23495=CARTESIAN_POINT('',(0.,0.,0.));
#23496=CARTESIAN_POINT('',(0.,0.,0.));
#23497=CARTESIAN_POINT('',(38.7298334620742,-3.,6.));
#23498=CARTESIAN_POINT('',(38.7298334620742,3.,6.));
#23499=CARTESIAN_POINT('',(39.7298334620742,0.,3.));
#23500=CARTESIAN_POINT('',(38.7298334620742,-6.2,3.));
#23501=CARTESIAN_POINT('',(38.7298334620742,8.7,3.));
#23502=CARTESIAN_POINT('',(0.,0.,0.));
#23503=CARTESIAN_POINT('',(0.,0.,0.));
#23504=CARTESIAN_POINT('',(0.,0.,0.));
#23505=CARTESIAN_POINT('',(0.,0.,0.));
#23506=CARTESIAN_POINT('',(0.,0.,0.));
#23507=CARTESIAN_POINT('',(0.,0.,0.));
#23508=CARTESIAN_POINT('',(0.,0.,0.));
#23509=CARTESIAN_POINT('',(0.,0.,0.));
#23510=CARTESIAN_POINT('',(0.,0.,0.));
#23511=CARTESIAN_POINT('',(0.,0.,0.));
#23512=CARTESIAN_POINT('',(0.,0.,0.));
#23513=CARTESIAN_POINT('',(38.7298334620742,-3.,16.));
#23514=CARTESIAN_POINT('',(38.7298334620742,3.,16.));
#23515=CARTESIAN_POINT('',(39.7298334620742,0.,13.));
#23516=CARTESIAN_POINT('',(38.7298334620742,-7.7,13.));
#23517=CARTESIAN_POINT('',(38.7298334620742,6.7,13.));
#23518=CARTESIAN_POINT('',(0.,0.,0.));
#23519=CARTESIAN_POINT('',(0.,0.,0.));
#23520=CARTESIAN_POINT('',(0.,0.,0.));
#23521=CARTESIAN_POINT('',(0.,0.,0.));
#23522=CARTESIAN_POINT('',(0.,0.,0.));
#23523=CARTESIAN_POINT('',(0.,0.,0.));
#23524=CARTESIAN_POINT('',(0.,0.,0.));
#23525=CARTESIAN_POINT('',(0.,0.,0.));
#23526=CARTESIAN_POINT('',(0.,0.,0.));
#23527=CARTESIAN_POINT('',(0.,0.,0.));
#23528=CARTESIAN_POINT('',(0.,0.,0.));
#23529=CARTESIAN_POINT('',(0.,0.,0.));
#23530=CARTESIAN_POINT('',(0.,0.,0.));
#23531=CARTESIAN_POINT('',(0.,0.,0.));
#23532=CARTESIAN_POINT('',(0.,0.,0.));
#23533=CARTESIAN_POINT('',(0.,0.,0.));
#23534=CARTESIAN_POINT('',(19.3649167310371,-7.7,8.));
#23535=CARTESIAN_POINT('',(19.3649167310371,8.7,8.));
#23536=CARTESIAN_POINT('',(0.,0.,0.));
#23537=CARTESIAN_POINT('',(0.,0.,0.));
#23538=CARTESIAN_POINT('Origin',(18.056769185842,-5.6,6.69185245480489));
#23539=CARTESIAN_POINT('',(17.891769185842,-5.5,6.69185245480489));
#23540=CARTESIAN_POINT('Origin',(18.056769185842,-5.5,6.69185245480489));
#23541=CARTESIAN_POINT('',(17.891769185842,-4.5,6.69185245480489));
#23542=CARTESIAN_POINT('',(17.891769185842,-5.6,6.69185245480489));
#23543=CARTESIAN_POINT('Origin',(18.056769185842,-4.5,6.69185245480489));
#23544=CARTESIAN_POINT('Origin',(18.056769185842,-5.6,9.30814754519511));
#23545=CARTESIAN_POINT('',(17.891769185842,-5.5,9.30814754519511));
#23546=CARTESIAN_POINT('Origin',(18.056769185842,-5.5,9.30814754519511));
#23547=CARTESIAN_POINT('',(17.891769185842,-4.5,9.30814754519511));
#23548=CARTESIAN_POINT('',(17.891769185842,-5.6,9.30814754519511));
#23549=CARTESIAN_POINT('Origin',(18.056769185842,-4.5,9.30814754519511));
#23550=CARTESIAN_POINT('Origin',(20.6730642762322,-5.6,9.30814754519511));
#23551=CARTESIAN_POINT('',(20.5080642762322,-5.5,9.30814754519511));
#23552=CARTESIAN_POINT('Origin',(20.6730642762322,-5.5,9.30814754519511));
#23553=CARTESIAN_POINT('',(20.5080642762322,-4.5,9.30814754519511));
#23554=CARTESIAN_POINT('',(20.5080642762322,-5.6,9.30814754519511));
#23555=CARTESIAN_POINT('Origin',(20.6730642762322,-4.5,9.30814754519511));
#23556=CARTESIAN_POINT('Origin',(20.6730642762322,-5.6,6.69185245480489));
#23557=CARTESIAN_POINT('',(20.5080642762322,-5.5,6.69185245480489));
#23558=CARTESIAN_POINT('Origin',(20.6730642762322,-5.5,6.69185245480489));
#23559=CARTESIAN_POINT('',(20.5080642762322,-4.5,6.69185245480489));
#23560=CARTESIAN_POINT('',(20.5080642762322,-5.6,6.69185245480489));
#23561=CARTESIAN_POINT('Origin',(20.6730642762322,-4.5,6.69185245480489));
#23562=CARTESIAN_POINT('Origin',(19.3649167310371,-5.6,8.));
#23563=CARTESIAN_POINT('',(17.7649167310371,-5.5,8.));
#23564=CARTESIAN_POINT('Origin',(19.3649167310371,-5.5,8.));
#23565=CARTESIAN_POINT('',(17.7649167310371,-4.5,8.));
#23566=CARTESIAN_POINT('',(17.7649167310371,-5.6,8.));
#23567=CARTESIAN_POINT('Origin',(19.3649167310371,-4.5,8.));
#23568=CARTESIAN_POINT('Origin',(19.3649167310371,-5.5,8.));
#23569=CARTESIAN_POINT('',(17.2795596239014,-4.5,7.29908221900242));
#23570=CARTESIAN_POINT('',(17.2795596239014,-5.5,7.29908221900242));
#23571=CARTESIAN_POINT('',(17.2795596239014,-5.5,7.29908221900242));
#23572=CARTESIAN_POINT('',(20.8502738381728,-4.5,6.37712777327313));
#23573=CARTESIAN_POINT('Origin',(19.3649167310371,-4.5,8.));
#23574=CARTESIAN_POINT('',(20.8502738381728,-5.5,6.37712777327313));
#23575=CARTESIAN_POINT('',(20.8502738381728,-5.5,6.37712777327313));
#23576=CARTESIAN_POINT('Origin',(19.3649167310371,-5.5,8.));
#23577=CARTESIAN_POINT('Origin',(19.3649167310371,-5.5,8.));
#23578=CARTESIAN_POINT('',(17.8795596239014,-5.5,9.62287222672687));
#23579=CARTESIAN_POINT('',(17.8795596239014,-4.5,9.62287222672687));
#23580=CARTESIAN_POINT('',(17.8795596239014,-5.5,9.62287222672687));
#23581=CARTESIAN_POINT('',(21.4502738381728,-5.5,8.70091778099758));
#23582=CARTESIAN_POINT('Origin',(19.3649167310371,-5.5,8.));
#23583=CARTESIAN_POINT('',(21.4502738381728,-4.5,8.70091778099758));
#23584=CARTESIAN_POINT('',(21.4502738381728,-5.5,8.70091778099758));
#23585=CARTESIAN_POINT('Origin',(19.3649167310371,-4.5,8.));
#23586=CARTESIAN_POINT('Origin',(0.3,-5.5,14.1618950038622));
#23587=CARTESIAN_POINT('',(38.1584122091775,-5.5,4.38689500386223));
#23588=CARTESIAN_POINT('',(0.3,-5.5,14.1618950038622));
#23589=CARTESIAN_POINT('',(38.1584122091775,-4.5,4.38689500386223));
#23590=CARTESIAN_POINT('',(38.1584122091775,-5.5,4.38689500386223));
#23591=CARTESIAN_POINT('',(0.3,-4.5,14.1618950038622));
#23592=CARTESIAN_POINT('Origin',(19.3649167310371,-4.5,8.));
#23593=CARTESIAN_POINT('',(37.5584122091775,-4.5,2.06310499613778));
#23594=CARTESIAN_POINT('Origin',(38.7298334620742,-4.5,3.));
#23595=CARTESIAN_POINT('',(38.4298334620742,-4.5,1.83810499613777));
#23596=CARTESIAN_POINT('',(0.571421252896674,-4.5,11.6131049961378));
#23597=CARTESIAN_POINT('',(38.4298334620742,-4.5,1.83810499613777));
#23598=CARTESIAN_POINT('',(1.17142125289667,-4.5,13.9368950038622));
#23599=CARTESIAN_POINT('Origin',(0.,-4.5,13.));
#23600=CARTESIAN_POINT('',(0.3,-4.5,14.1618950038622));
#23601=CARTESIAN_POINT('',(-1.,-4.5,13.));
#23602=CARTESIAN_POINT('Origin',(0.,-4.5,13.));
#23603=CARTESIAN_POINT('',(37.7298334620742,-4.5,3.));
#23604=CARTESIAN_POINT('Origin',(38.7298334620742,-4.5,3.));
#23605=CARTESIAN_POINT('Origin',(38.4298334620742,-5.5,1.83810499613777));
#23606=CARTESIAN_POINT('',(37.5584122091775,-5.5,2.06310499613778));
#23607=CARTESIAN_POINT('',(37.5584122091775,-5.5,2.06310499613778));
#23608=CARTESIAN_POINT('',(38.4298334620742,-5.5,1.83810499613777));
#23609=CARTESIAN_POINT('Origin',(0.,-5.6,13.));
#23610=CARTESIAN_POINT('',(-1.,-5.5,13.));
#23611=CARTESIAN_POINT('Origin',(0.,-5.5,13.));
#23612=CARTESIAN_POINT('',(-1.,-5.6,13.));
#23613=CARTESIAN_POINT('Origin',(0.,-5.5,13.));
#23614=CARTESIAN_POINT('',(0.571421252896672,-5.5,11.6131049961378));
#23615=CARTESIAN_POINT('',(0.571421252896672,-5.5,11.6131049961378));
#23616=CARTESIAN_POINT('',(1.17142125289667,-5.5,13.9368950038622));
#23617=CARTESIAN_POINT('Origin',(0.,-5.5,13.));
#23618=CARTESIAN_POINT('',(1.17142125289667,-5.5,13.9368950038622));
#23619=CARTESIAN_POINT('Origin',(38.4298334620742,-5.5,1.83810499613777));
#23620=CARTESIAN_POINT('',(38.4298334620742,-5.5,1.83810499613777));
#23621=CARTESIAN_POINT('Origin',(38.7298334620742,-5.6,3.));
#23622=CARTESIAN_POINT('',(37.7298334620742,-5.5,3.));
#23623=CARTESIAN_POINT('Origin',(38.7298334620742,-5.5,3.));
#23624=CARTESIAN_POINT('',(37.7298334620742,-5.6,3.));
#23625=CARTESIAN_POINT('Origin',(38.7298334620742,-5.5,3.));
#23626=CARTESIAN_POINT('Origin',(38.7298334620742,-5.5,3.));
#23627=CARTESIAN_POINT('Origin',(0.3,-5.5,14.1618950038622));
#23628=CARTESIAN_POINT('',(0.3,-5.5,14.1618950038622));
#23629=CARTESIAN_POINT('Origin',(19.3649167310371,-5.5,8.));
#23630=CARTESIAN_POINT('',(0.,0.,0.));
#23631=CARTESIAN_POINT('Origin',(38.7298334620742,-5.5,3.));
#23632=CARTESIAN_POINT('',(38.1248334620742,-4.5,3.));
#23633=CARTESIAN_POINT('Origin',(38.7298334620742,-4.5,3.));
#23634=CARTESIAN_POINT('',(38.1248334620742,-5.5,3.));
#23635=CARTESIAN_POINT('',(38.1248334620742,-5.5,3.));
#23636=CARTESIAN_POINT('Origin',(38.7298334620742,-5.5,3.));
#23637=CARTESIAN_POINT('Origin',(38.7298334620742,-5.5,3.));
#23638=CARTESIAN_POINT('',(37.7298334620742,-4.5,3.));
#23639=CARTESIAN_POINT('Origin',(38.7298334620742,-4.5,3.));
#23640=CARTESIAN_POINT('',(37.7298334620742,-5.5,3.));
#23641=CARTESIAN_POINT('',(37.7298334620742,-5.5,3.));
#23642=CARTESIAN_POINT('Origin',(38.7298334620742,-5.5,3.));
#23643=CARTESIAN_POINT('Origin',(38.7298334620742,-4.5,3.));
#23644=CARTESIAN_POINT('Origin',(38.7298334620742,-5.5,3.));
#23645=CARTESIAN_POINT('',(0.,0.,0.));
#23646=CARTESIAN_POINT('Origin',(0.,-5.5,13.));
#23647=CARTESIAN_POINT('',(-0.605,-4.5,13.));
#23648=CARTESIAN_POINT('Origin',(0.,-4.5,13.));
#23649=CARTESIAN_POINT('',(-0.605,-5.5,13.));
#23650=CARTESIAN_POINT('',(-0.605,-5.5,13.));
#23651=CARTESIAN_POINT('Origin',(0.,-5.5,13.));
#23652=CARTESIAN_POINT('Origin',(0.,-5.5,13.));
#23653=CARTESIAN_POINT('',(-1.,-4.5,13.));
#23654=CARTESIAN_POINT('Origin',(0.,-4.5,13.));
#23655=CARTESIAN_POINT('',(-1.,-5.5,13.));
#23656=CARTESIAN_POINT('',(-1.,-5.5,13.));
#23657=CARTESIAN_POINT('Origin',(0.,-5.5,13.));
#23658=CARTESIAN_POINT('Origin',(0.,-4.5,13.));
#23659=CARTESIAN_POINT('Origin',(0.,-5.5,13.));
#23660=CARTESIAN_POINT('',(0.,0.,0.));
#23661=CARTESIAN_POINT('Origin',(18.056769185842,-5.9,6.69185245480489));
#23662=CARTESIAN_POINT('',(17.831769185842,-5.8,6.69185245480489));
#23663=CARTESIAN_POINT('Origin',(18.056769185842,-5.8,6.69185245480489));
#23664=CARTESIAN_POINT('',(17.831769185842,-5.5,6.69185245480489));
#23665=CARTESIAN_POINT('',(17.831769185842,-5.9,6.69185245480489));
#23666=CARTESIAN_POINT('Origin',(18.056769185842,-5.5,6.69185245480489));
#23667=CARTESIAN_POINT('Origin',(18.056769185842,-5.9,9.30814754519511));
#23668=CARTESIAN_POINT('',(17.831769185842,-5.8,9.30814754519511));
#23669=CARTESIAN_POINT('Origin',(18.056769185842,-5.8,9.30814754519511));
#23670=CARTESIAN_POINT('',(17.831769185842,-5.5,9.30814754519511));
#23671=CARTESIAN_POINT('',(17.831769185842,-5.9,9.30814754519511));
#23672=CARTESIAN_POINT('Origin',(18.056769185842,-5.5,9.30814754519511));
#23673=CARTESIAN_POINT('Origin',(20.6730642762322,-5.9,9.30814754519511));
#23674=CARTESIAN_POINT('',(20.4480642762322,-5.8,9.30814754519511));
#23675=CARTESIAN_POINT('Origin',(20.6730642762322,-5.8,9.30814754519511));
#23676=CARTESIAN_POINT('',(20.4480642762322,-5.5,9.30814754519511));
#23677=CARTESIAN_POINT('',(20.4480642762322,-5.9,9.30814754519511));
#23678=CARTESIAN_POINT('Origin',(20.6730642762322,-5.5,9.30814754519511));
#23679=CARTESIAN_POINT('Origin',(20.6730642762322,-5.9,6.69185245480489));
#23680=CARTESIAN_POINT('',(20.4480642762322,-5.8,6.69185245480489));
#23681=CARTESIAN_POINT('Origin',(20.6730642762322,-5.8,6.69185245480489));
#23682=CARTESIAN_POINT('',(20.4480642762322,-5.5,6.69185245480489));
#23683=CARTESIAN_POINT('',(20.4480642762322,-5.9,6.69185245480489));
#23684=CARTESIAN_POINT('Origin',(20.6730642762322,-5.5,6.69185245480489));
#23685=CARTESIAN_POINT('Origin',(19.3649167310371,-5.8,8.));
#23686=CARTESIAN_POINT('',(18.3449167310371,-5.5,8.));
#23687=CARTESIAN_POINT('Origin',(19.3649167310371,-5.5,8.));
#23688=CARTESIAN_POINT('',(18.3449167310371,-5.8,8.));
#23689=CARTESIAN_POINT('',(18.3449167310371,-5.8,8.));
#23690=CARTESIAN_POINT('Origin',(19.3649167310371,-5.8,8.));
#23691=CARTESIAN_POINT('Origin',(19.3649167310371,-5.8,8.));
#23692=CARTESIAN_POINT('',(17.1649167310371,-5.5,8.));
#23693=CARTESIAN_POINT('Origin',(19.3649167310371,-5.5,8.));
#23694=CARTESIAN_POINT('',(17.1649167310371,-5.8,8.));
#23695=CARTESIAN_POINT('',(17.1649167310371,-5.8,8.));
#23696=CARTESIAN_POINT('Origin',(19.3649167310371,-5.8,8.));
#23697=CARTESIAN_POINT('Origin',(19.3649167310371,-5.5,8.));
#23698=CARTESIAN_POINT('Origin',(19.3649167310371,-5.8,8.));
#23699=CARTESIAN_POINT('',(0.,0.,0.));
#23700=CARTESIAN_POINT('Origin',(20.6730642762322,-5.8,9.30814754519511));
#23701=CARTESIAN_POINT('',(20.3230642762322,-5.8,9.30814754519511));
#23702=CARTESIAN_POINT('Origin',(20.6730642762322,-5.8,9.30814754519511));
#23703=CARTESIAN_POINT('',(20.4730642762322,-5.8,9.30814754519511));
#23704=CARTESIAN_POINT('Origin',(20.6730642762322,-5.8,9.30814754519511));
#23705=CARTESIAN_POINT('Origin',(20.6730642762322,-5.9,9.30814754519511));
#23706=CARTESIAN_POINT('',(20.3230642762322,-5.9,9.30814754519511));
#23707=CARTESIAN_POINT('',(20.3230642762322,-5.9,9.30814754519511));
#23708=CARTESIAN_POINT('Origin',(20.6730642762322,-5.9,9.30814754519511));
#23709=CARTESIAN_POINT('Origin',(20.6730642762322,-5.9,9.30814754519511));
#23710=CARTESIAN_POINT('Origin',(20.6730642762322,-5.8,9.30814754519511));
#23711=CARTESIAN_POINT('',(20.4730642762322,-5.1,9.30814754519511));
#23712=CARTESIAN_POINT('Origin',(20.6730642762322,-5.1,9.30814754519511));
#23713=CARTESIAN_POINT('',(20.4730642762322,-5.8,9.30814754519511));
#23714=CARTESIAN_POINT('Origin',(20.6730642762322,-5.1,9.30814754519511));
#23715=CARTESIAN_POINT('',(0.,0.,0.));
#23716=CARTESIAN_POINT('Origin',(18.056769185842,-5.8,9.30814754519511));
#23717=CARTESIAN_POINT('',(17.706769185842,-5.8,9.30814754519511));
#23718=CARTESIAN_POINT('Origin',(18.056769185842,-5.8,9.30814754519511));
#23719=CARTESIAN_POINT('',(17.856769185842,-5.8,9.30814754519511));
#23720=CARTESIAN_POINT('Origin',(18.056769185842,-5.8,9.30814754519511));
#23721=CARTESIAN_POINT('Origin',(18.056769185842,-5.9,9.30814754519511));
#23722=CARTESIAN_POINT('',(17.706769185842,-5.9,9.30814754519511));
#23723=CARTESIAN_POINT('',(17.706769185842,-5.9,9.30814754519511));
#23724=CARTESIAN_POINT('Origin',(18.056769185842,-5.9,9.30814754519511));
#23725=CARTESIAN_POINT('Origin',(18.056769185842,-5.9,9.30814754519511));
#23726=CARTESIAN_POINT('Origin',(18.056769185842,-5.8,9.30814754519511));
#23727=CARTESIAN_POINT('',(17.856769185842,-5.1,9.30814754519511));
#23728=CARTESIAN_POINT('Origin',(18.056769185842,-5.1,9.30814754519511));
#23729=CARTESIAN_POINT('',(17.856769185842,-5.8,9.30814754519511));
#23730=CARTESIAN_POINT('Origin',(18.056769185842,-5.1,9.30814754519511));
#23731=CARTESIAN_POINT('',(0.,0.,0.));
#23732=CARTESIAN_POINT('Origin',(18.056769185842,-5.8,6.69185245480489));
#23733=CARTESIAN_POINT('',(17.706769185842,-5.8,6.69185245480489));
#23734=CARTESIAN_POINT('Origin',(18.056769185842,-5.8,6.69185245480489));
#23735=CARTESIAN_POINT('',(17.856769185842,-5.8,6.69185245480489));
#23736=CARTESIAN_POINT('Origin',(18.056769185842,-5.8,6.69185245480489));
#23737=CARTESIAN_POINT('Origin',(18.056769185842,-5.9,6.69185245480489));
#23738=CARTESIAN_POINT('',(17.706769185842,-5.9,6.69185245480489));
#23739=CARTESIAN_POINT('',(17.706769185842,-5.9,6.69185245480489));
#23740=CARTESIAN_POINT('Origin',(18.056769185842,-5.9,6.69185245480489));
#23741=CARTESIAN_POINT('Origin',(18.056769185842,-5.9,6.69185245480489));
#23742=CARTESIAN_POINT('Origin',(18.056769185842,-5.8,6.69185245480489));
#23743=CARTESIAN_POINT('',(17.856769185842,-5.1,6.69185245480489));
#23744=CARTESIAN_POINT('Origin',(18.056769185842,-5.1,6.69185245480489));
#23745=CARTESIAN_POINT('',(17.856769185842,-5.8,6.69185245480489));
#23746=CARTESIAN_POINT('Origin',(18.056769185842,-5.1,6.69185245480489));
#23747=CARTESIAN_POINT('',(0.,0.,0.));
#23748=CARTESIAN_POINT('Origin',(20.6730642762322,-5.8,6.69185245480489));
#23749=CARTESIAN_POINT('',(20.3230642762322,-5.8,6.69185245480489));
#23750=CARTESIAN_POINT('Origin',(20.6730642762322,-5.8,6.69185245480489));
#23751=CARTESIAN_POINT('',(20.4730642762322,-5.8,6.69185245480489));
#23752=CARTESIAN_POINT('Origin',(20.6730642762322,-5.8,6.69185245480489));
#23753=CARTESIAN_POINT('Origin',(20.6730642762322,-5.9,6.69185245480489));
#23754=CARTESIAN_POINT('',(20.3230642762322,-5.9,6.69185245480489));
#23755=CARTESIAN_POINT('',(20.3230642762322,-5.9,6.69185245480489));
#23756=CARTESIAN_POINT('Origin',(20.6730642762322,-5.9,6.69185245480489));
#23757=CARTESIAN_POINT('Origin',(20.6730642762322,-5.9,6.69185245480489));
#23758=CARTESIAN_POINT('Origin',(20.6730642762322,-5.8,6.69185245480489));
#23759=CARTESIAN_POINT('',(20.4730642762322,-5.1,6.69185245480489));
#23760=CARTESIAN_POINT('Origin',(20.6730642762322,-5.1,6.69185245480489));
#23761=CARTESIAN_POINT('',(20.4730642762322,-5.8,6.69185245480489));
#23762=CARTESIAN_POINT('Origin',(20.6730642762322,-5.1,6.69185245480489));
#23763=CARTESIAN_POINT('',(0.,0.,0.));
#23764=CARTESIAN_POINT('Origin',(18.056769185842,-4.6,6.69185245480489));
#23765=CARTESIAN_POINT('',(17.831769185842,-4.5,6.69185245480489));
#23766=CARTESIAN_POINT('Origin',(18.056769185842,-4.5,6.69185245480489));
#23767=CARTESIAN_POINT('',(17.831769185842,-4.2,6.69185245480489));
#23768=CARTESIAN_POINT('',(17.831769185842,-4.6,6.69185245480489));
#23769=CARTESIAN_POINT('Origin',(18.056769185842,-4.2,6.69185245480489));
#23770=CARTESIAN_POINT('Origin',(18.056769185842,-4.6,9.30814754519511));
#23771=CARTESIAN_POINT('',(17.831769185842,-4.5,9.30814754519511));
#23772=CARTESIAN_POINT('Origin',(18.056769185842,-4.5,9.30814754519511));
#23773=CARTESIAN_POINT('',(17.831769185842,-4.2,9.30814754519511));
#23774=CARTESIAN_POINT('',(17.831769185842,-4.6,9.30814754519511));
#23775=CARTESIAN_POINT('Origin',(18.056769185842,-4.2,9.30814754519511));
#23776=CARTESIAN_POINT('Origin',(20.6730642762322,-4.6,9.30814754519511));
#23777=CARTESIAN_POINT('',(20.4480642762322,-4.5,9.30814754519511));
#23778=CARTESIAN_POINT('Origin',(20.6730642762322,-4.5,9.30814754519511));
#23779=CARTESIAN_POINT('',(20.4480642762322,-4.2,9.30814754519511));
#23780=CARTESIAN_POINT('',(20.4480642762322,-4.6,9.30814754519511));
#23781=CARTESIAN_POINT('Origin',(20.6730642762322,-4.2,9.30814754519511));
#23782=CARTESIAN_POINT('Origin',(20.6730642762322,-4.6,6.69185245480489));
#23783=CARTESIAN_POINT('',(20.4480642762322,-4.5,6.69185245480489));
#23784=CARTESIAN_POINT('Origin',(20.6730642762322,-4.5,6.69185245480489));
#23785=CARTESIAN_POINT('',(20.4480642762322,-4.2,6.69185245480489));
#23786=CARTESIAN_POINT('',(20.4480642762322,-4.6,6.69185245480489));
#23787=CARTESIAN_POINT('Origin',(20.6730642762322,-4.2,6.69185245480489));
#23788=CARTESIAN_POINT('Origin',(19.3649167310371,-4.5,8.));
#23789=CARTESIAN_POINT('',(18.3449167310371,-4.2,8.));
#23790=CARTESIAN_POINT('Origin',(19.3649167310371,-4.2,8.));
#23791=CARTESIAN_POINT('',(18.3449167310371,-4.5,8.));
#23792=CARTESIAN_POINT('',(18.3449167310371,-4.5,8.));
#23793=CARTESIAN_POINT('Origin',(19.3649167310371,-4.5,8.));
#23794=CARTESIAN_POINT('Origin',(19.3649167310371,-4.5,8.));
#23795=CARTESIAN_POINT('',(17.1649167310371,-4.2,8.));
#23796=CARTESIAN_POINT('Origin',(19.3649167310371,-4.2,8.));
#23797=CARTESIAN_POINT('',(17.1649167310371,-4.5,8.));
#23798=CARTESIAN_POINT('',(17.1649167310371,-4.5,8.));
#23799=CARTESIAN_POINT('Origin',(19.3649167310371,-4.5,8.));
#23800=CARTESIAN_POINT('Origin',(19.3649167310371,-4.2,8.));
#23801=CARTESIAN_POINT('Origin',(19.3649167310371,-4.5,8.));
#23802=CARTESIAN_POINT('',(0.,0.,0.));
#23803=CARTESIAN_POINT('Origin',(20.6730642762322,-4.2,9.30814754519511));
#23804=CARTESIAN_POINT('',(20.3230642762322,-4.2,9.30814754519511));
#23805=CARTESIAN_POINT('Origin',(20.6730642762322,-4.2,9.30814754519511));
#23806=CARTESIAN_POINT('',(20.4730642762322,-4.2,9.30814754519511));
#23807=CARTESIAN_POINT('Origin',(20.6730642762322,-4.2,9.30814754519511));
#23808=CARTESIAN_POINT('Origin',(20.6730642762322,-4.2,9.30814754519511));
#23809=CARTESIAN_POINT('',(20.3230642762322,-4.1,9.30814754519511));
#23810=CARTESIAN_POINT('Origin',(20.6730642762322,-4.1,9.30814754519511));
#23811=CARTESIAN_POINT('',(20.3230642762322,-4.2,9.30814754519511));
#23812=CARTESIAN_POINT('Origin',(20.6730642762322,-4.1,9.30814754519511));
#23813=CARTESIAN_POINT('Origin',(20.6730642762322,-4.9,9.30814754519511));
#23814=CARTESIAN_POINT('',(20.4730642762322,-4.9,9.30814754519511));
#23815=CARTESIAN_POINT('',(20.4730642762322,-4.9,9.30814754519511));
#23816=CARTESIAN_POINT('Origin',(20.6730642762322,-4.9,9.30814754519511));
#23817=CARTESIAN_POINT('Origin',(20.6730642762322,-4.9,9.30814754519511));
#23818=CARTESIAN_POINT('',(0.,0.,0.));
#23819=CARTESIAN_POINT('Origin',(18.056769185842,-4.2,9.30814754519511));
#23820=CARTESIAN_POINT('',(17.706769185842,-4.2,9.30814754519511));
#23821=CARTESIAN_POINT('Origin',(18.056769185842,-4.2,9.30814754519511));
#23822=CARTESIAN_POINT('',(17.856769185842,-4.2,9.30814754519511));
#23823=CARTESIAN_POINT('Origin',(18.056769185842,-4.2,9.30814754519511));
#23824=CARTESIAN_POINT('Origin',(18.056769185842,-4.2,9.30814754519511));
#23825=CARTESIAN_POINT('',(17.706769185842,-4.1,9.30814754519511));
#23826=CARTESIAN_POINT('Origin',(18.056769185842,-4.1,9.30814754519511));
#23827=CARTESIAN_POINT('',(17.706769185842,-4.2,9.30814754519511));
#23828=CARTESIAN_POINT('Origin',(18.056769185842,-4.1,9.30814754519511));
#23829=CARTESIAN_POINT('Origin',(18.056769185842,-4.9,9.30814754519511));
#23830=CARTESIAN_POINT('',(17.856769185842,-4.9,9.30814754519511));
#23831=CARTESIAN_POINT('',(17.856769185842,-4.9,9.30814754519511));
#23832=CARTESIAN_POINT('Origin',(18.056769185842,-4.9,9.30814754519511));
#23833=CARTESIAN_POINT('Origin',(18.056769185842,-4.9,9.30814754519511));
#23834=CARTESIAN_POINT('',(0.,0.,0.));
#23835=CARTESIAN_POINT('Origin',(18.056769185842,-4.2,6.69185245480489));
#23836=CARTESIAN_POINT('',(17.706769185842,-4.2,6.69185245480489));
#23837=CARTESIAN_POINT('Origin',(18.056769185842,-4.2,6.69185245480489));
#23838=CARTESIAN_POINT('',(17.856769185842,-4.2,6.69185245480489));
#23839=CARTESIAN_POINT('Origin',(18.056769185842,-4.2,6.69185245480489));
#23840=CARTESIAN_POINT('Origin',(18.056769185842,-4.2,6.69185245480489));
#23841=CARTESIAN_POINT('',(17.706769185842,-4.1,6.69185245480489));
#23842=CARTESIAN_POINT('Origin',(18.056769185842,-4.1,6.69185245480489));
#23843=CARTESIAN_POINT('',(17.706769185842,-4.2,6.69185245480489));
#23844=CARTESIAN_POINT('Origin',(18.056769185842,-4.1,6.69185245480489));
#23845=CARTESIAN_POINT('Origin',(18.056769185842,-4.9,6.69185245480489));
#23846=CARTESIAN_POINT('',(17.856769185842,-4.9,6.69185245480489));
#23847=CARTESIAN_POINT('',(17.856769185842,-4.9,6.69185245480489));
#23848=CARTESIAN_POINT('Origin',(18.056769185842,-4.9,6.69185245480489));
#23849=CARTESIAN_POINT('Origin',(18.056769185842,-4.9,6.69185245480489));
#23850=CARTESIAN_POINT('',(0.,0.,0.));
#23851=CARTESIAN_POINT('Origin',(20.6730642762322,-4.2,6.69185245480489));
#23852=CARTESIAN_POINT('',(20.3230642762322,-4.2,6.69185245480489));
#23853=CARTESIAN_POINT('Origin',(20.6730642762322,-4.2,6.69185245480489));
#23854=CARTESIAN_POINT('',(20.4730642762322,-4.2,6.69185245480489));
#23855=CARTESIAN_POINT('Origin',(20.6730642762322,-4.2,6.69185245480489));
#23856=CARTESIAN_POINT('Origin',(20.6730642762322,-4.2,6.69185245480489));
#23857=CARTESIAN_POINT('',(20.3230642762322,-4.1,6.69185245480489));
#23858=CARTESIAN_POINT('Origin',(20.6730642762322,-4.1,6.69185245480489));
#23859=CARTESIAN_POINT('',(20.3230642762322,-4.2,6.69185245480489));
#23860=CARTESIAN_POINT('Origin',(20.6730642762322,-4.1,6.69185245480489));
#23861=CARTESIAN_POINT('Origin',(20.6730642762322,-4.9,6.69185245480489));
#23862=CARTESIAN_POINT('',(20.4730642762322,-4.9,6.69185245480489));
#23863=CARTESIAN_POINT('',(20.4730642762322,-4.9,6.69185245480489));
#23864=CARTESIAN_POINT('Origin',(20.6730642762322,-4.9,6.69185245480489));
#23865=CARTESIAN_POINT('Origin',(20.6730642762322,-4.9,6.69185245480489));
#23866=CARTESIAN_POINT('',(0.,0.,0.));
#23867=CARTESIAN_POINT('Origin',(18.056769185842,6.9,6.69185245480489));
#23868=CARTESIAN_POINT('',(17.891769185842,7.,6.69185245480489));
#23869=CARTESIAN_POINT('Origin',(18.056769185842,7.,6.69185245480489));
#23870=CARTESIAN_POINT('',(17.891769185842,8.,6.69185245480489));
#23871=CARTESIAN_POINT('',(17.891769185842,6.9,6.69185245480489));
#23872=CARTESIAN_POINT('Origin',(18.056769185842,8.,6.69185245480489));
#23873=CARTESIAN_POINT('Origin',(18.056769185842,6.9,9.30814754519511));
#23874=CARTESIAN_POINT('',(17.891769185842,7.,9.30814754519511));
#23875=CARTESIAN_POINT('Origin',(18.056769185842,7.,9.30814754519511));
#23876=CARTESIAN_POINT('',(17.891769185842,8.,9.30814754519511));
#23877=CARTESIAN_POINT('',(17.891769185842,6.9,9.30814754519511));
#23878=CARTESIAN_POINT('Origin',(18.056769185842,8.,9.30814754519511));
#23879=CARTESIAN_POINT('Origin',(20.6730642762322,6.9,9.30814754519511));
#23880=CARTESIAN_POINT('',(20.5080642762322,7.,9.30814754519511));
#23881=CARTESIAN_POINT('Origin',(20.6730642762322,7.,9.30814754519511));
#23882=CARTESIAN_POINT('',(20.5080642762322,8.,9.30814754519511));
#23883=CARTESIAN_POINT('',(20.5080642762322,6.9,9.30814754519511));
#23884=CARTESIAN_POINT('Origin',(20.6730642762322,8.,9.30814754519511));
#23885=CARTESIAN_POINT('Origin',(20.6730642762322,6.9,6.69185245480489));
#23886=CARTESIAN_POINT('',(20.5080642762322,7.,6.69185245480489));
#23887=CARTESIAN_POINT('Origin',(20.6730642762322,7.,6.69185245480489));
#23888=CARTESIAN_POINT('',(20.5080642762322,8.,6.69185245480489));
#23889=CARTESIAN_POINT('',(20.5080642762322,6.9,6.69185245480489));
#23890=CARTESIAN_POINT('Origin',(20.6730642762322,8.,6.69185245480489));
#23891=CARTESIAN_POINT('Origin',(19.3649167310371,6.9,8.));
#23892=CARTESIAN_POINT('',(17.7649167310371,7.,8.));
#23893=CARTESIAN_POINT('Origin',(19.3649167310371,7.,8.));
#23894=CARTESIAN_POINT('',(17.7649167310371,8.,8.));
#23895=CARTESIAN_POINT('',(17.7649167310371,6.9,8.));
#23896=CARTESIAN_POINT('Origin',(19.3649167310371,8.,8.));
#23897=CARTESIAN_POINT('Origin',(19.3649167310371,7.,8.));
#23898=CARTESIAN_POINT('',(17.2795596239014,8.,7.29908221900242));
#23899=CARTESIAN_POINT('',(17.2795596239014,7.,7.29908221900242));
#23900=CARTESIAN_POINT('',(17.2795596239014,7.,7.29908221900242));
#23901=CARTESIAN_POINT('',(20.8502738381728,8.,6.37712777327313));
#23902=CARTESIAN_POINT('Origin',(19.3649167310371,8.,8.));
#23903=CARTESIAN_POINT('',(20.8502738381728,7.,6.37712777327313));
#23904=CARTESIAN_POINT('',(20.8502738381728,7.,6.37712777327313));
#23905=CARTESIAN_POINT('Origin',(19.3649167310371,7.,8.));
#23906=CARTESIAN_POINT('Origin',(19.3649167310371,7.,8.));
#23907=CARTESIAN_POINT('',(17.8795596239014,7.,9.62287222672687));
#23908=CARTESIAN_POINT('',(17.8795596239014,8.,9.62287222672687));
#23909=CARTESIAN_POINT('',(17.8795596239014,7.,9.62287222672687));
#23910=CARTESIAN_POINT('',(21.4502738381728,7.,8.70091778099758));
#23911=CARTESIAN_POINT('Origin',(19.3649167310371,7.,8.));
#23912=CARTESIAN_POINT('',(21.4502738381728,8.,8.70091778099758));
#23913=CARTESIAN_POINT('',(21.4502738381728,7.,8.70091778099758));
#23914=CARTESIAN_POINT('Origin',(19.3649167310371,8.,8.));
#23915=CARTESIAN_POINT('Origin',(0.3,7.,14.1618950038622));
#23916=CARTESIAN_POINT('',(38.1584122091775,7.,4.38689500386223));
#23917=CARTESIAN_POINT('',(0.3,7.,14.1618950038622));
#23918=CARTESIAN_POINT('',(38.1584122091775,8.,4.38689500386223));
#23919=CARTESIAN_POINT('',(38.1584122091775,7.,4.38689500386223));
#23920=CARTESIAN_POINT('',(0.3,8.,14.1618950038622));
#23921=CARTESIAN_POINT('Origin',(19.3649167310371,8.,8.));
#23922=CARTESIAN_POINT('',(37.5584122091775,8.,2.06310499613778));
#23923=CARTESIAN_POINT('Origin',(38.7298334620742,8.,3.));
#23924=CARTESIAN_POINT('',(38.4298334620742,8.,1.83810499613777));
#23925=CARTESIAN_POINT('',(0.571421252896674,8.,11.6131049961378));
#23926=CARTESIAN_POINT('',(38.4298334620742,8.,1.83810499613777));
#23927=CARTESIAN_POINT('',(1.17142125289667,8.,13.9368950038622));
#23928=CARTESIAN_POINT('Origin',(0.,8.,13.));
#23929=CARTESIAN_POINT('',(0.3,8.,14.1618950038622));
#23930=CARTESIAN_POINT('',(-1.,8.,13.));
#23931=CARTESIAN_POINT('Origin',(0.,8.,13.));
#23932=CARTESIAN_POINT('',(37.7298334620742,8.,3.));
#23933=CARTESIAN_POINT('Origin',(38.7298334620742,8.,3.));
#23934=CARTESIAN_POINT('Origin',(38.4298334620742,7.,1.83810499613777));
#23935=CARTESIAN_POINT('',(37.5584122091775,7.,2.06310499613778));
#23936=CARTESIAN_POINT('',(37.5584122091775,7.,2.06310499613778));
#23937=CARTESIAN_POINT('',(38.4298334620742,7.,1.83810499613777));
#23938=CARTESIAN_POINT('Origin',(0.,6.9,13.));
#23939=CARTESIAN_POINT('',(-1.,7.,13.));
#23940=CARTESIAN_POINT('Origin',(0.,7.,13.));
#23941=CARTESIAN_POINT('',(-1.,6.9,13.));
#23942=CARTESIAN_POINT('Origin',(0.,7.,13.));
#23943=CARTESIAN_POINT('',(0.571421252896672,7.,11.6131049961378));
#23944=CARTESIAN_POINT('',(0.571421252896672,7.,11.6131049961378));
#23945=CARTESIAN_POINT('',(1.17142125289667,7.,13.9368950038622));
#23946=CARTESIAN_POINT('Origin',(0.,7.,13.));
#23947=CARTESIAN_POINT('',(1.17142125289667,7.,13.9368950038622));
#23948=CARTESIAN_POINT('Origin',(38.4298334620742,7.,1.83810499613777));
#23949=CARTESIAN_POINT('',(38.4298334620742,7.,1.83810499613777));
#23950=CARTESIAN_POINT('Origin',(38.7298334620742,6.9,3.));
#23951=CARTESIAN_POINT('',(37.7298334620742,7.,3.));
#23952=CARTESIAN_POINT('Origin',(38.7298334620742,7.,3.));
#23953=CARTESIAN_POINT('',(37.7298334620742,6.9,3.));
#23954=CARTESIAN_POINT('Origin',(38.7298334620742,7.,3.));
#23955=CARTESIAN_POINT('Origin',(38.7298334620742,7.,3.));
#23956=CARTESIAN_POINT('Origin',(0.3,7.,14.1618950038622));
#23957=CARTESIAN_POINT('',(0.3,7.,14.1618950038622));
#23958=CARTESIAN_POINT('Origin',(19.3649167310371,7.,8.));
#23959=CARTESIAN_POINT('',(0.,0.,0.));
#23960=CARTESIAN_POINT('Origin',(38.7298334620742,7.,3.));
#23961=CARTESIAN_POINT('',(38.1248334620742,8.,3.));
#23962=CARTESIAN_POINT('Origin',(38.7298334620742,8.,3.));
#23963=CARTESIAN_POINT('',(38.1248334620742,7.,3.));
#23964=CARTESIAN_POINT('',(38.1248334620742,7.,3.));
#23965=CARTESIAN_POINT('Origin',(38.7298334620742,7.,3.));
#23966=CARTESIAN_POINT('Origin',(38.7298334620742,7.,3.));
#23967=CARTESIAN_POINT('',(37.7298334620742,8.,3.));
#23968=CARTESIAN_POINT('Origin',(38.7298334620742,8.,3.));
#23969=CARTESIAN_POINT('',(37.7298334620742,7.,3.));
#23970=CARTESIAN_POINT('',(37.7298334620742,7.,3.));
#23971=CARTESIAN_POINT('Origin',(38.7298334620742,7.,3.));
#23972=CARTESIAN_POINT('Origin',(38.7298334620742,8.,3.));
#23973=CARTESIAN_POINT('Origin',(38.7298334620742,7.,3.));
#23974=CARTESIAN_POINT('',(0.,0.,0.));
#23975=CARTESIAN_POINT('Origin',(0.,7.,13.));
#23976=CARTESIAN_POINT('',(-0.605,8.,13.));
#23977=CARTESIAN_POINT('Origin',(0.,8.,13.));
#23978=CARTESIAN_POINT('',(-0.605,7.,13.));
#23979=CARTESIAN_POINT('',(-0.605,7.,13.));
#23980=CARTESIAN_POINT('Origin',(0.,7.,13.));
#23981=CARTESIAN_POINT('Origin',(0.,7.,13.));
#23982=CARTESIAN_POINT('',(-1.,8.,13.));
#23983=CARTESIAN_POINT('Origin',(0.,8.,13.));
#23984=CARTESIAN_POINT('',(-1.,7.,13.));
#23985=CARTESIAN_POINT('',(-1.,7.,13.));
#23986=CARTESIAN_POINT('Origin',(0.,7.,13.));
#23987=CARTESIAN_POINT('Origin',(0.,8.,13.));
#23988=CARTESIAN_POINT('Origin',(0.,7.,13.));
#23989=CARTESIAN_POINT('',(0.,0.,0.));
#23990=CARTESIAN_POINT('Origin',(18.056769185842,6.6,6.69185245480489));
#23991=CARTESIAN_POINT('',(17.831769185842,6.7,6.69185245480489));
#23992=CARTESIAN_POINT('Origin',(18.056769185842,6.7,6.69185245480489));
#23993=CARTESIAN_POINT('',(17.831769185842,7.,6.69185245480489));
#23994=CARTESIAN_POINT('',(17.831769185842,6.6,6.69185245480489));
#23995=CARTESIAN_POINT('Origin',(18.056769185842,7.,6.69185245480489));
#23996=CARTESIAN_POINT('Origin',(18.056769185842,6.6,9.30814754519511));
#23997=CARTESIAN_POINT('',(17.831769185842,6.7,9.30814754519511));
#23998=CARTESIAN_POINT('Origin',(18.056769185842,6.7,9.30814754519511));
#23999=CARTESIAN_POINT('',(17.831769185842,7.,9.30814754519511));
#24000=CARTESIAN_POINT('',(17.831769185842,6.6,9.30814754519511));
#24001=CARTESIAN_POINT('Origin',(18.056769185842,7.,9.30814754519511));
#24002=CARTESIAN_POINT('Origin',(20.6730642762322,6.6,9.30814754519511));
#24003=CARTESIAN_POINT('',(20.4480642762322,6.7,9.30814754519511));
#24004=CARTESIAN_POINT('Origin',(20.6730642762322,6.7,9.30814754519511));
#24005=CARTESIAN_POINT('',(20.4480642762322,7.,9.30814754519511));
#24006=CARTESIAN_POINT('',(20.4480642762322,6.6,9.30814754519511));
#24007=CARTESIAN_POINT('Origin',(20.6730642762322,7.,9.30814754519511));
#24008=CARTESIAN_POINT('Origin',(20.6730642762322,6.6,6.69185245480489));
#24009=CARTESIAN_POINT('',(20.4480642762322,6.7,6.69185245480489));
#24010=CARTESIAN_POINT('Origin',(20.6730642762322,6.7,6.69185245480489));
#24011=CARTESIAN_POINT('',(20.4480642762322,7.,6.69185245480489));
#24012=CARTESIAN_POINT('',(20.4480642762322,6.6,6.69185245480489));
#24013=CARTESIAN_POINT('Origin',(20.6730642762322,7.,6.69185245480489));
#24014=CARTESIAN_POINT('Origin',(19.3649167310371,6.7,8.));
#24015=CARTESIAN_POINT('',(18.3449167310371,7.,8.));
#24016=CARTESIAN_POINT('Origin',(19.3649167310371,7.,8.));
#24017=CARTESIAN_POINT('',(18.3449167310371,6.7,8.));
#24018=CARTESIAN_POINT('',(18.3449167310371,6.7,8.));
#24019=CARTESIAN_POINT('Origin',(19.3649167310371,6.7,8.));
#24020=CARTESIAN_POINT('Origin',(19.3649167310371,6.7,8.));
#24021=CARTESIAN_POINT('',(17.1649167310371,7.,8.));
#24022=CARTESIAN_POINT('Origin',(19.3649167310371,7.,8.));
#24023=CARTESIAN_POINT('',(17.1649167310371,6.7,8.));
#24024=CARTESIAN_POINT('',(17.1649167310371,6.7,8.));
#24025=CARTESIAN_POINT('Origin',(19.3649167310371,6.7,8.));
#24026=CARTESIAN_POINT('Origin',(19.3649167310371,7.,8.));
#24027=CARTESIAN_POINT('Origin',(19.3649167310371,6.7,8.));
#24028=CARTESIAN_POINT('',(0.,0.,0.));
#24029=CARTESIAN_POINT('Origin',(20.6730642762322,6.7,9.30814754519511));
#24030=CARTESIAN_POINT('',(20.3230642762322,6.7,9.30814754519511));
#24031=CARTESIAN_POINT('Origin',(20.6730642762322,6.7,9.30814754519511));
#24032=CARTESIAN_POINT('',(20.4730642762322,6.7,9.30814754519511));
#24033=CARTESIAN_POINT('Origin',(20.6730642762322,6.7,9.30814754519511));
#24034=CARTESIAN_POINT('Origin',(20.6730642762322,6.6,9.30814754519511));
#24035=CARTESIAN_POINT('',(20.3230642762322,6.6,9.30814754519511));
#24036=CARTESIAN_POINT('',(20.3230642762322,6.6,9.30814754519511));
#24037=CARTESIAN_POINT('Origin',(20.6730642762322,6.6,9.30814754519511));
#24038=CARTESIAN_POINT('Origin',(20.6730642762322,6.6,9.30814754519511));
#24039=CARTESIAN_POINT('Origin',(20.6730642762322,6.7,9.30814754519511));
#24040=CARTESIAN_POINT('',(20.4730642762322,7.4,9.30814754519511));
#24041=CARTESIAN_POINT('Origin',(20.6730642762322,7.4,9.30814754519511));
#24042=CARTESIAN_POINT('',(20.4730642762322,6.7,9.30814754519511));
#24043=CARTESIAN_POINT('Origin',(20.6730642762322,7.4,9.30814754519511));
#24044=CARTESIAN_POINT('',(0.,0.,0.));
#24045=CARTESIAN_POINT('Origin',(18.056769185842,6.7,9.30814754519511));
#24046=CARTESIAN_POINT('',(17.706769185842,6.7,9.30814754519511));
#24047=CARTESIAN_POINT('Origin',(18.056769185842,6.7,9.30814754519511));
#24048=CARTESIAN_POINT('',(17.856769185842,6.7,9.30814754519511));
#24049=CARTESIAN_POINT('Origin',(18.056769185842,6.7,9.30814754519511));
#24050=CARTESIAN_POINT('Origin',(18.056769185842,6.6,9.30814754519511));
#24051=CARTESIAN_POINT('',(17.706769185842,6.6,9.30814754519511));
#24052=CARTESIAN_POINT('',(17.706769185842,6.6,9.30814754519511));
#24053=CARTESIAN_POINT('Origin',(18.056769185842,6.6,9.30814754519511));
#24054=CARTESIAN_POINT('Origin',(18.056769185842,6.6,9.30814754519511));
#24055=CARTESIAN_POINT('Origin',(18.056769185842,6.7,9.30814754519511));
#24056=CARTESIAN_POINT('',(17.856769185842,7.4,9.30814754519511));
#24057=CARTESIAN_POINT('Origin',(18.056769185842,7.4,9.30814754519511));
#24058=CARTESIAN_POINT('',(17.856769185842,6.7,9.30814754519511));
#24059=CARTESIAN_POINT('Origin',(18.056769185842,7.4,9.30814754519511));
#24060=CARTESIAN_POINT('',(0.,0.,0.));
#24061=CARTESIAN_POINT('Origin',(18.056769185842,6.7,6.69185245480489));
#24062=CARTESIAN_POINT('',(17.706769185842,6.7,6.69185245480489));
#24063=CARTESIAN_POINT('Origin',(18.056769185842,6.7,6.69185245480489));
#24064=CARTESIAN_POINT('',(17.856769185842,6.7,6.69185245480489));
#24065=CARTESIAN_POINT('Origin',(18.056769185842,6.7,6.69185245480489));
#24066=CARTESIAN_POINT('Origin',(18.056769185842,6.6,6.69185245480489));
#24067=CARTESIAN_POINT('',(17.706769185842,6.6,6.69185245480489));
#24068=CARTESIAN_POINT('',(17.706769185842,6.6,6.69185245480489));
#24069=CARTESIAN_POINT('Origin',(18.056769185842,6.6,6.69185245480489));
#24070=CARTESIAN_POINT('Origin',(18.056769185842,6.6,6.69185245480489));
#24071=CARTESIAN_POINT('Origin',(18.056769185842,6.7,6.69185245480489));
#24072=CARTESIAN_POINT('',(17.856769185842,7.4,6.69185245480489));
#24073=CARTESIAN_POINT('Origin',(18.056769185842,7.4,6.69185245480489));
#24074=CARTESIAN_POINT('',(17.856769185842,6.7,6.69185245480489));
#24075=CARTESIAN_POINT('Origin',(18.056769185842,7.4,6.69185245480489));
#24076=CARTESIAN_POINT('',(0.,0.,0.));
#24077=CARTESIAN_POINT('Origin',(20.6730642762322,6.7,6.69185245480489));
#24078=CARTESIAN_POINT('',(20.3230642762322,6.7,6.69185245480489));
#24079=CARTESIAN_POINT('Origin',(20.6730642762322,6.7,6.69185245480489));
#24080=CARTESIAN_POINT('',(20.4730642762322,6.7,6.69185245480489));
#24081=CARTESIAN_POINT('Origin',(20.6730642762322,6.7,6.69185245480489));
#24082=CARTESIAN_POINT('Origin',(20.6730642762322,6.6,6.69185245480489));
#24083=CARTESIAN_POINT('',(20.3230642762322,6.6,6.69185245480489));
#24084=CARTESIAN_POINT('',(20.3230642762322,6.6,6.69185245480489));
#24085=CARTESIAN_POINT('Origin',(20.6730642762322,6.6,6.69185245480489));
#24086=CARTESIAN_POINT('Origin',(20.6730642762322,6.6,6.69185245480489));
#24087=CARTESIAN_POINT('Origin',(20.6730642762322,6.7,6.69185245480489));
#24088=CARTESIAN_POINT('',(20.4730642762322,7.4,6.69185245480489));
#24089=CARTESIAN_POINT('Origin',(20.6730642762322,7.4,6.69185245480489));
#24090=CARTESIAN_POINT('',(20.4730642762322,6.7,6.69185245480489));
#24091=CARTESIAN_POINT('Origin',(20.6730642762322,7.4,6.69185245480489));
#24092=CARTESIAN_POINT('',(0.,0.,0.));
#24093=CARTESIAN_POINT('Origin',(18.056769185842,7.9,6.69185245480489));
#24094=CARTESIAN_POINT('',(17.831769185842,8.,6.69185245480489));
#24095=CARTESIAN_POINT('Origin',(18.056769185842,8.,6.69185245480489));
#24096=CARTESIAN_POINT('',(17.831769185842,8.3,6.69185245480489));
#24097=CARTESIAN_POINT('',(17.831769185842,7.9,6.69185245480489));
#24098=CARTESIAN_POINT('Origin',(18.056769185842,8.3,6.69185245480489));
#24099=CARTESIAN_POINT('Origin',(18.056769185842,7.9,9.30814754519511));
#24100=CARTESIAN_POINT('',(17.831769185842,8.,9.30814754519511));
#24101=CARTESIAN_POINT('Origin',(18.056769185842,8.,9.30814754519511));
#24102=CARTESIAN_POINT('',(17.831769185842,8.3,9.30814754519511));
#24103=CARTESIAN_POINT('',(17.831769185842,7.9,9.30814754519511));
#24104=CARTESIAN_POINT('Origin',(18.056769185842,8.3,9.30814754519511));
#24105=CARTESIAN_POINT('Origin',(20.6730642762322,7.9,9.30814754519511));
#24106=CARTESIAN_POINT('',(20.4480642762322,8.,9.30814754519511));
#24107=CARTESIAN_POINT('Origin',(20.6730642762322,8.,9.30814754519511));
#24108=CARTESIAN_POINT('',(20.4480642762322,8.3,9.30814754519511));
#24109=CARTESIAN_POINT('',(20.4480642762322,7.9,9.30814754519511));
#24110=CARTESIAN_POINT('Origin',(20.6730642762322,8.3,9.30814754519511));
#24111=CARTESIAN_POINT('Origin',(20.6730642762322,7.9,6.69185245480489));
#24112=CARTESIAN_POINT('',(20.4480642762322,8.,6.69185245480489));
#24113=CARTESIAN_POINT('Origin',(20.6730642762322,8.,6.69185245480489));
#24114=CARTESIAN_POINT('',(20.4480642762322,8.3,6.69185245480489));
#24115=CARTESIAN_POINT('',(20.4480642762322,7.9,6.69185245480489));
#24116=CARTESIAN_POINT('Origin',(20.6730642762322,8.3,6.69185245480489));
#24117=CARTESIAN_POINT('Origin',(19.3649167310371,8.,8.));
#24118=CARTESIAN_POINT('',(18.3449167310371,8.3,8.));
#24119=CARTESIAN_POINT('Origin',(19.3649167310371,8.3,8.));
#24120=CARTESIAN_POINT('',(18.3449167310371,8.,8.));
#24121=CARTESIAN_POINT('',(18.3449167310371,8.,8.));
#24122=CARTESIAN_POINT('Origin',(19.3649167310371,8.,8.));
#24123=CARTESIAN_POINT('Origin',(19.3649167310371,8.,8.));
#24124=CARTESIAN_POINT('',(17.1649167310371,8.3,8.));
#24125=CARTESIAN_POINT('Origin',(19.3649167310371,8.3,8.));
#24126=CARTESIAN_POINT('',(17.1649167310371,8.,8.));
#24127=CARTESIAN_POINT('',(17.1649167310371,8.,8.));
#24128=CARTESIAN_POINT('Origin',(19.3649167310371,8.,8.));
#24129=CARTESIAN_POINT('Origin',(19.3649167310371,8.3,8.));
#24130=CARTESIAN_POINT('Origin',(19.3649167310371,8.,8.));
#24131=CARTESIAN_POINT('',(0.,0.,0.));
#24132=CARTESIAN_POINT('Origin',(20.6730642762322,8.3,9.30814754519511));
#24133=CARTESIAN_POINT('',(20.3230642762322,8.3,9.30814754519511));
#24134=CARTESIAN_POINT('Origin',(20.6730642762322,8.3,9.30814754519511));
#24135=CARTESIAN_POINT('',(20.4730642762322,8.3,9.30814754519511));
#24136=CARTESIAN_POINT('Origin',(20.6730642762322,8.3,9.30814754519511));
#24137=CARTESIAN_POINT('Origin',(20.6730642762322,8.3,9.30814754519511));
#24138=CARTESIAN_POINT('',(20.3230642762322,8.4,9.30814754519511));
#24139=CARTESIAN_POINT('Origin',(20.6730642762322,8.4,9.30814754519511));
#24140=CARTESIAN_POINT('',(20.3230642762322,8.3,9.30814754519511));
#24141=CARTESIAN_POINT('Origin',(20.6730642762322,8.4,9.30814754519511));
#24142=CARTESIAN_POINT('Origin',(20.6730642762322,7.6,9.30814754519511));
#24143=CARTESIAN_POINT('',(20.4730642762322,7.6,9.30814754519511));
#24144=CARTESIAN_POINT('',(20.4730642762322,7.6,9.30814754519511));
#24145=CARTESIAN_POINT('Origin',(20.6730642762322,7.6,9.30814754519511));
#24146=CARTESIAN_POINT('Origin',(20.6730642762322,7.6,9.30814754519511));
#24147=CARTESIAN_POINT('',(0.,0.,0.));
#24148=CARTESIAN_POINT('Origin',(18.056769185842,8.3,9.30814754519511));
#24149=CARTESIAN_POINT('',(17.706769185842,8.3,9.30814754519511));
#24150=CARTESIAN_POINT('Origin',(18.056769185842,8.3,9.30814754519511));
#24151=CARTESIAN_POINT('',(17.856769185842,8.3,9.30814754519511));
#24152=CARTESIAN_POINT('Origin',(18.056769185842,8.3,9.30814754519511));
#24153=CARTESIAN_POINT('Origin',(18.056769185842,8.3,9.30814754519511));
#24154=CARTESIAN_POINT('',(17.706769185842,8.4,9.30814754519511));
#24155=CARTESIAN_POINT('Origin',(18.056769185842,8.4,9.30814754519511));
#24156=CARTESIAN_POINT('',(17.706769185842,8.3,9.30814754519511));
#24157=CARTESIAN_POINT('Origin',(18.056769185842,8.4,9.30814754519511));
#24158=CARTESIAN_POINT('Origin',(18.056769185842,7.6,9.30814754519511));
#24159=CARTESIAN_POINT('',(17.856769185842,7.6,9.30814754519511));
#24160=CARTESIAN_POINT('',(17.856769185842,7.6,9.30814754519511));
#24161=CARTESIAN_POINT('Origin',(18.056769185842,7.6,9.30814754519511));
#24162=CARTESIAN_POINT('Origin',(18.056769185842,7.6,9.30814754519511));
#24163=CARTESIAN_POINT('',(0.,0.,0.));
#24164=CARTESIAN_POINT('Origin',(18.056769185842,8.3,6.69185245480489));
#24165=CARTESIAN_POINT('',(17.706769185842,8.3,6.69185245480489));
#24166=CARTESIAN_POINT('Origin',(18.056769185842,8.3,6.69185245480489));
#24167=CARTESIAN_POINT('',(17.856769185842,8.3,6.69185245480489));
#24168=CARTESIAN_POINT('Origin',(18.056769185842,8.3,6.69185245480489));
#24169=CARTESIAN_POINT('Origin',(18.056769185842,8.3,6.69185245480489));
#24170=CARTESIAN_POINT('',(17.706769185842,8.4,6.69185245480489));
#24171=CARTESIAN_POINT('Origin',(18.056769185842,8.4,6.69185245480489));
#24172=CARTESIAN_POINT('',(17.706769185842,8.3,6.69185245480489));
#24173=CARTESIAN_POINT('Origin',(18.056769185842,8.4,6.69185245480489));
#24174=CARTESIAN_POINT('Origin',(18.056769185842,7.6,6.69185245480489));
#24175=CARTESIAN_POINT('',(17.856769185842,7.6,6.69185245480489));
#24176=CARTESIAN_POINT('',(17.856769185842,7.6,6.69185245480489));
#24177=CARTESIAN_POINT('Origin',(18.056769185842,7.6,6.69185245480489));
#24178=CARTESIAN_POINT('Origin',(18.056769185842,7.6,6.69185245480489));
#24179=CARTESIAN_POINT('',(0.,0.,0.));
#24180=CARTESIAN_POINT('Origin',(20.6730642762322,8.3,6.69185245480489));
#24181=CARTESIAN_POINT('',(20.3230642762322,8.3,6.69185245480489));
#24182=CARTESIAN_POINT('Origin',(20.6730642762322,8.3,6.69185245480489));
#24183=CARTESIAN_POINT('',(20.4730642762322,8.3,6.69185245480489));
#24184=CARTESIAN_POINT('Origin',(20.6730642762322,8.3,6.69185245480489));
#24185=CARTESIAN_POINT('Origin',(20.6730642762322,8.3,6.69185245480489));
#24186=CARTESIAN_POINT('',(20.3230642762322,8.4,6.69185245480489));
#24187=CARTESIAN_POINT('Origin',(20.6730642762322,8.4,6.69185245480489));
#24188=CARTESIAN_POINT('',(20.3230642762322,8.3,6.69185245480489));
#24189=CARTESIAN_POINT('Origin',(20.6730642762322,8.4,6.69185245480489));
#24190=CARTESIAN_POINT('Origin',(20.6730642762322,7.6,6.69185245480489));
#24191=CARTESIAN_POINT('',(20.4730642762322,7.6,6.69185245480489));
#24192=CARTESIAN_POINT('',(20.4730642762322,7.6,6.69185245480489));
#24193=CARTESIAN_POINT('Origin',(20.6730642762322,7.6,6.69185245480489));
#24194=CARTESIAN_POINT('Origin',(20.6730642762322,7.6,6.69185245480489));
#24195=CARTESIAN_POINT('',(0.,0.,0.));
#24196=CARTESIAN_POINT('',(0.,0.,0.));
#24197=CARTESIAN_POINT('Origin',(0.,0.,0.));
#24198=CARTESIAN_POINT('',(-1.070235,-0.308121667383195,-1.31065986708547E-16));
#24199=CARTESIAN_POINT('',(-1.31065986708547E-16,-0.308121667383195,1.070235));
#24200=CARTESIAN_POINT('Origin',(0.,-0.308121667383195,0.));
#24201=CARTESIAN_POINT('Origin',(0.,-0.308121667383195,0.));
#24202=CARTESIAN_POINT('',(-1.31065986708547E-16,0.308121667383195,1.070235));
#24203=CARTESIAN_POINT('Origin',(-1.34711147906209E-16,0.,1.1));
#24204=CARTESIAN_POINT('',(-1.070235,0.308121667383195,1.31065986708547E-16));
#24205=CARTESIAN_POINT('Origin',(0.,0.308121667383195,0.));
#24206=CARTESIAN_POINT('Origin',(0.,0.308121667383195,0.));
#24207=CARTESIAN_POINT('Origin',(0.,0.,0.));
#24208=CARTESIAN_POINT('',(-1.070235,0.5,-1.31065986708547E-16));
#24209=CARTESIAN_POINT('',(-1.070235,0.,-1.31065986708547E-16));
#24210=CARTESIAN_POINT('Origin',(0.,0.5,0.));
#24211=CARTESIAN_POINT('Origin',(0.,0.,0.));
#24212=CARTESIAN_POINT('',(-0.6,-0.44,-7.34788079488412E-17));
#24213=CARTESIAN_POINT('Origin',(0.,-0.44,0.));
#24214=CARTESIAN_POINT('',(-0.6,0.44,-7.34788079488412E-17));
#24215=CARTESIAN_POINT('',(-0.6,0.,-7.34788079488412E-17));
#24216=CARTESIAN_POINT('Origin',(0.,0.44,0.));
#24217=CARTESIAN_POINT('Origin',(0.,0.47,0.));
#24218=CARTESIAN_POINT('',(-0.66,0.5,-8.08266887437253E-17));
#24219=CARTESIAN_POINT('',(-0.63,0.47,-7.71527483462832E-17));
#24220=CARTESIAN_POINT('Origin',(0.,0.5,0.));
#24221=CARTESIAN_POINT('Origin',(1.070235,0.5,0.));
#24222=CARTESIAN_POINT('Origin',(0.,0.,0.));
#24223=CARTESIAN_POINT('',(-1.070235,-0.5,-1.31065986708547E-16));
#24224=CARTESIAN_POINT('Origin',(0.,-0.5,0.));
#24225=CARTESIAN_POINT('',(-1.070235,0.,-1.31065986708547E-16));
#24226=CARTESIAN_POINT('Origin',(0.66,-0.5,0.));
#24227=CARTESIAN_POINT('',(-0.66,-0.5,-8.08266887437253E-17));
#24228=CARTESIAN_POINT('Origin',(0.,-0.5,0.));
#24229=CARTESIAN_POINT('Origin',(0.,-0.47,0.));
#24230=CARTESIAN_POINT('',(-0.63,-0.47,-7.71527483462832E-17));
#24231=CARTESIAN_POINT('',(0.,0.,0.));
#24232=CARTESIAN_POINT('Origin',(0.,0.,0.));
#24233=CARTESIAN_POINT('',(-1.129765,0.308121667383195,-1.38356309103871E-16));
#24234=CARTESIAN_POINT('',(-1.38356309103871E-16,0.308121667383195,1.129765));
#24235=CARTESIAN_POINT('Origin',(0.,0.308121667383195,0.));
#24236=CARTESIAN_POINT('Origin',(0.,0.308121667383195,0.));
#24237=CARTESIAN_POINT('',(-1.38356309103871E-16,-0.308121667383195,1.129765));
#24238=CARTESIAN_POINT('Origin',(-1.34711147906209E-16,0.,1.1));
#24239=CARTESIAN_POINT('',(-1.129765,-0.308121667383195,1.38356309103871E-16));
#24240=CARTESIAN_POINT('Origin',(0.,-0.308121667383195,0.));
#24241=CARTESIAN_POINT('Origin',(0.,-0.308121667383195,0.));
#24242=CARTESIAN_POINT('Origin',(0.,0.,0.));
#24243=CARTESIAN_POINT('',(-1.129765,-0.5,-1.38356309103871E-16));
#24244=CARTESIAN_POINT('Origin',(0.,-0.5,0.));
#24245=CARTESIAN_POINT('',(-1.129765,0.,-1.38356309103871E-16));
#24246=CARTESIAN_POINT('Origin',(1.54,0.5,0.));
#24247=CARTESIAN_POINT('',(-1.54,0.5,-1.88595607068692E-16));
#24248=CARTESIAN_POINT('Origin',(0.,0.5,0.));
#24249=CARTESIAN_POINT('',(-1.129765,0.5,-1.38356309103871E-16));
#24250=CARTESIAN_POINT('Origin',(0.,0.5,0.));
#24251=CARTESIAN_POINT('Origin',(0.,0.47,0.));
#24252=CARTESIAN_POINT('',(-1.6,0.44,-1.95943487863577E-16));
#24253=CARTESIAN_POINT('Origin',(0.,0.44,0.));
#24254=CARTESIAN_POINT('',(-1.57,0.47,-1.92269547466134E-16));
#24255=CARTESIAN_POINT('Origin',(0.,0.,0.));
#24256=CARTESIAN_POINT('',(-1.6,-0.44,-1.95943487863577E-16));
#24257=CARTESIAN_POINT('Origin',(0.,-0.44,0.));
#24258=CARTESIAN_POINT('',(-1.6,0.,-1.95943487863577E-16));
#24259=CARTESIAN_POINT('Origin',(0.,-0.47,0.));
#24260=CARTESIAN_POINT('',(-1.54,-0.5,-1.88595607068692E-16));
#24261=CARTESIAN_POINT('Origin',(0.,-0.5,0.));
#24262=CARTESIAN_POINT('',(-1.57,-0.47,-1.92269547466134E-16));
#24263=CARTESIAN_POINT('Origin',(1.129765,-0.5,0.));
#24264=CARTESIAN_POINT('Origin',(0.,0.,0.));
#24265=CARTESIAN_POINT('',(-1.129765,0.,-1.38356309103871E-16));
#24266=CARTESIAN_POINT('',(0.,0.,0.));
#24267=CARTESIAN_POINT('Origin',(1.1,0.,0.));
#24268=CARTESIAN_POINT('',(1.1,-2.23201749654651E-33,0.29765));
#24269=CARTESIAN_POINT('',(1.1,-2.23201749654651E-33,-0.29765));
#24270=CARTESIAN_POINT('Origin',(1.1,0.,0.));
#24271=CARTESIAN_POINT('Origin',(0.685838782044607,0.,-0.860014630714833));
#24272=CARTESIAN_POINT('',(0.918550922801216,-5.31350540756609E-33,-0.674432891191581));
#24273=CARTESIAN_POINT('',(0.453126641287998,8.49470414473068E-34,-1.04559637023808));
#24274=CARTESIAN_POINT('Origin',(0.685838782044607,0.,-0.860014630714833));
#24275=CARTESIAN_POINT('Origin',(-0.244773027351946,0.,-1.07242070340001));
#24276=CARTESIAN_POINT('',(0.0454142657089739,-2.23201749654651E-33,-1.1386540593921));
#24277=CARTESIAN_POINT('',(-0.534960320412865,-2.23201749654651E-33,-1.00618734740791));
#24278=CARTESIAN_POINT('Origin',(-0.244773027351946,0.,-1.07242070340001));
#24279=CARTESIAN_POINT('Origin',(-0.991065754692661,0.,-0.477272113029314));
#24280=CARTESIAN_POINT('',(-0.86192025974432,8.49470414473067E-34,-0.745445496560469));
#24281=CARTESIAN_POINT('',(-1.120211249641,-5.31350540756609E-33,-0.209098729498159));
#24282=CARTESIAN_POINT('Origin',(-0.991065754692661,0.,-0.477272113029314));
#24283=CARTESIAN_POINT('Origin',(-0.991065754692661,0.,0.477272113029314));
#24284=CARTESIAN_POINT('',(-1.120211249641,-2.23201749654651E-33,0.209098729498159));
#24285=CARTESIAN_POINT('',(-0.86192025974432,-2.23201749654651E-33,0.745445496560469));
#24286=CARTESIAN_POINT('Origin',(-0.991065754692661,0.,0.477272113029314));
#24287=CARTESIAN_POINT('Origin',(-0.244773027351946,0.,1.07242070340001));
#24288=CARTESIAN_POINT('',(-0.534960320412866,-2.23201749654651E-33,1.00618734740791));
#24289=CARTESIAN_POINT('',(0.0454142657089737,-2.23201749654651E-33,1.1386540593921));
#24290=CARTESIAN_POINT('Origin',(-0.244773027351946,0.,1.07242070340001));
#24291=CARTESIAN_POINT('Origin',(0.685838782044607,0.,0.860014630714833));
#24292=CARTESIAN_POINT('',(0.453126641287998,-2.23201749654651E-33,1.04559637023808));
#24293=CARTESIAN_POINT('',(0.918550922801216,-2.23201749654651E-33,0.674432891191581));
#24294=CARTESIAN_POINT('Origin',(0.685838782044607,0.,0.860014630714833));
#24295=CARTESIAN_POINT('',(0.,0.,0.));
#24296=CARTESIAN_POINT('Origin',(-0.244773027351946,0.,-1.07242070340001));
#24297=CARTESIAN_POINT('',(-0.0491413193775444,-0.17859,-0.890289804925809));
#24298=CARTESIAN_POINT('',(-0.120823405150736,-0.22859,-0.883420913717115));
#24299=CARTESIAN_POINT('Ctrl Pts',(-0.0491413193775443,-0.17859,-0.890289804925809));
#24300=CARTESIAN_POINT('Ctrl Pts',(-0.0622366108032282,-0.192197739766234,
-0.889566984227727));
#24301=CARTESIAN_POINT('Ctrl Pts',(-0.0768612314186783,-0.204076596372851,
-0.888465811801874));
#24302=CARTESIAN_POINT('Ctrl Pts',(-0.101256149639299,-0.219236411496476,
-0.885920360302595));
#24303=CARTESIAN_POINT('Ctrl Pts',(-0.110791504359706,-0.224284758603913,
-0.884792953245369));
#24304=CARTESIAN_POINT('Ctrl Pts',(-0.120823405150736,-0.22859,-0.883420913717114));
#24305=CARTESIAN_POINT('',(-0.110717377488918,-0.17859,-1.30366194557752));
#24306=CARTESIAN_POINT('Origin',(-0.244773027351946,-0.17859,-1.07242070340001));
#24307=CARTESIAN_POINT('',(-0.197287840980438,-0.22859,-1.29339487931037));
#24308=CARTESIAN_POINT('Ctrl Pts',(-0.197287840980438,-0.228590000000001,
-1.29339487931037));
#24309=CARTESIAN_POINT('Ctrl Pts',(-0.182957777157794,-0.223500193956903,
-1.2955807139676));
#24310=CARTESIAN_POINT('Ctrl Pts',(-0.169262868734191,-0.217292055674527,
-1.29742089529918));
#24311=CARTESIAN_POINT('Ctrl Pts',(-0.141475557257539,-0.202063936711524,
-1.30077481170484));
#24312=CARTESIAN_POINT('Ctrl Pts',(-0.12509796078425,-0.190965925779192,
-1.30244063166664));
#24313=CARTESIAN_POINT('Ctrl Pts',(-0.110717377488918,-0.178589999999999,
-1.30366194557752));
#24314=CARTESIAN_POINT('Origin',(-0.244773027351946,-0.22859,-1.07242070340001));
#24315=CARTESIAN_POINT('Origin',(0.891645,-0.22859,0.));
#24316=CARTESIAN_POINT('',(0.738933209129743,-0.22859,-1.07970853403602));
#24317=CARTESIAN_POINT('Origin',(0.,-0.22859,0.));
#24318=CARTESIAN_POINT('',(0.492160095813005,-0.22859,-0.743511429713312));
#24319=CARTESIAN_POINT('Origin',(0.685838782044607,-0.22859,-0.860014630714833));
#24320=CARTESIAN_POINT('Origin',(0.,-0.22859,0.));
#24321=CARTESIAN_POINT('Origin',(0.,-0.20359,0.));
#24322=CARTESIAN_POINT('',(0.665390629745762,-0.17859,-1.12652035750427));
#24323=CARTESIAN_POINT('Origin',(0.,-0.17859,0.));
#24324=CARTESIAN_POINT('Ctrl Pts',(0.665390629745762,-0.178589999999999,
-1.12652035750427));
#24325=CARTESIAN_POINT('Ctrl Pts',(0.677817179350845,-0.190965925779192,
-1.11918049044176));
#24326=CARTESIAN_POINT('Ctrl Pts',(0.691850111710621,-0.202063936711525,
-1.11057366572105));
#24327=CARTESIAN_POINT('Ctrl Pts',(0.715430404483016,-0.217292055674528,
-1.09549542885049));
#24328=CARTESIAN_POINT('Ctrl Pts',(0.726970665864658,-0.223500193956903,
-1.08789548468573));
#24329=CARTESIAN_POINT('Ctrl Pts',(0.738933209129742,-0.228590000000001,
-1.07970853403602));
#24330=CARTESIAN_POINT('Origin',(1.308355,-0.17859,0.));
#24331=CARTESIAN_POINT('',(0.430557068346269,-0.17859,-0.780801778252372));
#24332=CARTESIAN_POINT('Origin',(0.,-0.17859,0.));
#24333=CARTESIAN_POINT('Origin',(0.685838782044607,-0.17859,-0.860014630714833));
#24334=CARTESIAN_POINT('Origin',(0.,-0.20359,0.));
#24335=CARTESIAN_POINT('Ctrl Pts',(0.492160095813005,-0.22859,-0.743511429713312));
#24336=CARTESIAN_POINT('Ctrl Pts',(0.483716971155137,-0.224284758603913,
-0.74910027323947));
#24337=CARTESIAN_POINT('Ctrl Pts',(0.475615076997141,-0.219236411496476,
-0.754253267259386));
#24338=CARTESIAN_POINT('Ctrl Pts',(0.454740445159586,-0.204076596372851,
-0.767131198148022));
#24339=CARTESIAN_POINT('Ctrl Pts',(0.442041898089724,-0.192197739766234,
-0.774468705297715));
#24340=CARTESIAN_POINT('Ctrl Pts',(0.430557068346269,-0.17859,-0.780801778252372));
#24341=CARTESIAN_POINT('Origin',(0.685838782044607,0.,-0.860014630714833));
#24342=CARTESIAN_POINT('Origin',(-0.991065754692661,0.,0.477272113029314));
#24343=CARTESIAN_POINT('',(-0.834385970030061,-0.22859,0.314373756923179));
#24344=CARTESIAN_POINT('',(-1.21706609467953,-0.22859,0.480148859424376));
#24345=CARTESIAN_POINT('Origin',(-0.991065754692661,-0.22859,0.477272113029314));
#24346=CARTESIAN_POINT('',(-0.857033408469345,-0.17859,0.246017362786485));
#24347=CARTESIAN_POINT('Ctrl Pts',(-0.857033408469345,-0.17859,0.246017362786485));
#24348=CARTESIAN_POINT('Ctrl Pts',(-0.853414733916809,-0.192197739766234,
0.25862348517872));
#24349=CARTESIAN_POINT('Ctrl Pts',(-0.849086885944613,-0.204076596372852,
0.272636402105144));
#24350=CARTESIAN_POINT('Ctrl Pts',(-0.84117687424262,-0.219236411496476,
0.29585327254886));
#24351=CARTESIAN_POINT('Ctrl Pts',(-0.837955917596151,-0.224284758603913,
0.304898684347016));
#24352=CARTESIAN_POINT('Ctrl Pts',(-0.834385970030061,-0.22859,0.314373756923179));
#24353=CARTESIAN_POINT('',(-1.24633948454876,-0.17859,0.398033535370734));
#24354=CARTESIAN_POINT('Origin',(-0.991065754692661,-0.17859,0.477272113029314));
#24355=CARTESIAN_POINT('Ctrl Pts',(-1.21706609467953,-0.228590000000001,
0.480148859424375));
#24356=CARTESIAN_POINT('Ctrl Pts',(-1.22238586508374,-0.223500193956903,
0.466664474189734));
#24357=CARTESIAN_POINT('Ctrl Pts',(-1.22722731304024,-0.217292055674528,
0.453722404581342));
#24358=CARTESIAN_POINT('Ctrl Pts',(-1.23668039826116,-0.202063936711525,
0.427378095629262));
#24359=CARTESIAN_POINT('Ctrl Pts',(-1.24194881070179,-0.190965925779192,
0.411781799506707));
#24360=CARTESIAN_POINT('Ctrl Pts',(-1.24633948454876,-0.178589999999999,
0.398033535370735));
#24361=CARTESIAN_POINT('Origin',(1.308355,-0.17859,0.));
#24362=CARTESIAN_POINT('',(-0.857033408469345,-0.17859,-0.246017362786486));
#24363=CARTESIAN_POINT('Origin',(0.,-0.17859,0.));
#24364=CARTESIAN_POINT('',(-1.24633948454876,-0.17859,-0.398033535370734));
#24365=CARTESIAN_POINT('Origin',(-0.991065754692661,-0.17859,-0.477272113029314));
#24366=CARTESIAN_POINT('Origin',(0.,-0.17859,0.));
#24367=CARTESIAN_POINT('Origin',(0.,-0.20359,0.));
#24368=CARTESIAN_POINT('',(-1.21706609467953,-0.22859,-0.480148859424376));
#24369=CARTESIAN_POINT('Ctrl Pts',(-1.24633948454876,-0.178589999999999,
-0.398033535370735));
#24370=CARTESIAN_POINT('Ctrl Pts',(-1.24194881070179,-0.190965925779192,
-0.411781799506707));
#24371=CARTESIAN_POINT('Ctrl Pts',(-1.23668039826116,-0.202063936711525,
-0.427378095629262));
#24372=CARTESIAN_POINT('Ctrl Pts',(-1.22722731304024,-0.217292055674528,
-0.453722404581342));
#24373=CARTESIAN_POINT('Ctrl Pts',(-1.22238586508374,-0.223500193956903,
-0.466664474189735));
#24374=CARTESIAN_POINT('Ctrl Pts',(-1.21706609467953,-0.228590000000001,
-0.480148859424376));
#24375=CARTESIAN_POINT('Origin',(0.,-0.22859,0.));
#24376=CARTESIAN_POINT('Origin',(0.,-0.20359,0.));
#24377=CARTESIAN_POINT('',(-0.834385970030061,-0.22859,-0.314373756923179));
#24378=CARTESIAN_POINT('Origin',(0.,-0.22859,0.));
#24379=CARTESIAN_POINT('Ctrl Pts',(-0.834385970030061,-0.22859,-0.314373756923179));
#24380=CARTESIAN_POINT('Ctrl Pts',(-0.837955917596151,-0.224284758603913,
-0.304898684347017));
#24381=CARTESIAN_POINT('Ctrl Pts',(-0.84117687424262,-0.219236411496476,
-0.29585327254886));
#24382=CARTESIAN_POINT('Ctrl Pts',(-0.849086885944613,-0.204076596372851,
-0.272636402105144));
#24383=CARTESIAN_POINT('Ctrl Pts',(-0.853414733916809,-0.192197739766234,
-0.25862348517872));
#24384=CARTESIAN_POINT('Ctrl Pts',(-0.857033408469345,-0.17859,-0.246017362786486));
#24385=CARTESIAN_POINT('Origin',(0.891645,-0.22859,0.));
#24386=CARTESIAN_POINT('Origin',(-0.991065754692661,-0.22859,-0.477272113029314));
#24387=CARTESIAN_POINT('Origin',(-0.991065754692661,0.,-0.477272113029314));
#24388=CARTESIAN_POINT('Origin',(-0.244773027351946,0.,1.07242070340001));
#24389=CARTESIAN_POINT('',(-0.342007470572634,-0.17859,0.823445017045771));
#24390=CARTESIAN_POINT('',(-0.274443842703457,-0.22859,0.848358051312746));
#24391=CARTESIAN_POINT('Ctrl Pts',(-0.342007470572634,-0.17859,0.82344501704577));
#24392=CARTESIAN_POINT('Ctrl Pts',(-0.329895400534788,-0.192197739766234,
0.828475612108333));
#24393=CARTESIAN_POINT('Ctrl Pts',(-0.316241291845841,-0.204076596372851,
0.833828875110254));
#24394=CARTESIAN_POINT('Ctrl Pts',(-0.293157799979787,-0.219236411496476,
0.842120060887678));
#24395=CARTESIAN_POINT('Ctrl Pts',(-0.284077578642798,-0.224284758603913,
0.845241537587566));
#24396=CARTESIAN_POINT('Ctrl Pts',(-0.274443842703457,-0.22859,0.848358051312746));
#24397=CARTESIAN_POINT('',(-0.465884809239132,-0.17859,1.22259729696463));
#24398=CARTESIAN_POINT('Origin',(-0.244773027351946,-0.17859,1.07242070340001));
#24399=CARTESIAN_POINT('',(-0.383432803651627,-0.22859,1.25090850629007));
#24400=CARTESIAN_POINT('Ctrl Pts',(-0.383432803651627,-0.228590000000001,
1.25090850629007));
#24401=CARTESIAN_POINT('Ctrl Pts',(-0.397292143145055,-0.223500193956903,
1.24666029359345));
#24402=CARTESIAN_POINT('Ctrl Pts',(-0.410429254040296,-0.217292055674528,
1.2423762416108));
#24403=CARTESIAN_POINT('Ctrl Pts',(-0.436919966394242,-0.202063936711525,
1.23334155327433));
#24404=CARTESIAN_POINT('Ctrl Pts',(-0.45239844314147,-0.190965925779192,
1.22773643240386));
#24405=CARTESIAN_POINT('Ctrl Pts',(-0.465884809239131,-0.178589999999999,
1.22259729696463));
#24406=CARTESIAN_POINT('Origin',(-0.244773027351946,-0.22859,1.07242070340001));
#24407=CARTESIAN_POINT('Origin',(0.,-0.20359,0.));
#24408=CARTESIAN_POINT('',(-1.08827510730092,-0.17859,0.726257596761768));
#24409=CARTESIAN_POINT('Origin',(0.,-0.17859,0.));
#24410=CARTESIAN_POINT('',(-1.13422379278981,-0.22859,0.652172671839668));
#24411=CARTESIAN_POINT('Ctrl Pts',(-1.08827510730092,-0.178589999999999,
0.726257596761768));
#24412=CARTESIAN_POINT('Ctrl Pts',(-1.09628639266483,-0.190965925779192,
0.714252927236921));
#24413=CARTESIAN_POINT('Ctrl Pts',(-1.10519526655462,-0.202063936711525,
0.700409784949026));
#24414=CARTESIAN_POINT('Ctrl Pts',(-1.11989817444587,-0.217292055674528,
0.676593657348219));
#24415=CARTESIAN_POINT('Ctrl Pts',(-1.1269980984869,-0.223500193956903,
0.664739212499319));
#24416=CARTESIAN_POINT('Ctrl Pts',(-1.13422379278981,-0.228590000000001,
0.652172671839668));
#24417=CARTESIAN_POINT('Origin',(0.,-0.22859,0.));
#24418=CARTESIAN_POINT('Origin',(0.891645,-0.22859,0.));
#24419=CARTESIAN_POINT('',(-0.766018443552043,-0.22859,0.456340388485509));
#24420=CARTESIAN_POINT('Origin',(-0.991065754692661,-0.22859,0.477272113029314));
#24421=CARTESIAN_POINT('Origin',(0.,-0.22859,0.));
#24422=CARTESIAN_POINT('Origin',(1.308355,-0.17859,0.));
#24423=CARTESIAN_POINT('',(-0.7266957094931,-0.17859,0.516666383490662));
#24424=CARTESIAN_POINT('Origin',(0.,-0.17859,0.));
#24425=CARTESIAN_POINT('Origin',(-0.991065754692661,-0.17859,0.477272113029314));
#24426=CARTESIAN_POINT('Origin',(0.,-0.20359,0.));
#24427=CARTESIAN_POINT('Ctrl Pts',(-0.766018443552043,-0.22859,0.45634038848551));
#24428=CARTESIAN_POINT('Ctrl Pts',(-0.760836359413957,-0.224284758603913,
0.465039097006547));
#24429=CARTESIAN_POINT('Ctrl Pts',(-0.755772605319574,-0.219236411496476,
0.473197064326185));
#24430=CARTESIAN_POINT('Ctrl Pts',(-0.742552736711071,-0.204076596372852,
0.493856842454225));
#24431=CARTESIAN_POINT('Ctrl Pts',(-0.734295366171442,-0.192197739766234,
0.505977401048143));
#24432=CARTESIAN_POINT('Ctrl Pts',(-0.7266957094931,-0.17859,0.516666383490662));
#24433=CARTESIAN_POINT('Origin',(-0.991065754692661,0.,0.477272113029314));
#24434=CARTESIAN_POINT('Origin',(0.685838782044607,0.,0.860014630714833));
#24435=CARTESIAN_POINT('',(0.665417486529536,-0.17859,0.593506844649423));
#24436=CARTESIAN_POINT('',(0.950212795795148,-0.17859,0.899382259516035));
#24437=CARTESIAN_POINT('Origin',(0.685838782044607,-0.17859,0.860014630714833));
#24438=CARTESIAN_POINT('',(0.615354121677383,-0.22859,0.645267472417181));
#24439=CARTESIAN_POINT('Ctrl Pts',(0.615354121677383,-0.22859,0.64526747241718));
#24440=CARTESIAN_POINT('Ctrl Pts',(0.622681613212229,-0.224284758603913,
0.638279669203371));
#24441=CARTESIAN_POINT('Ctrl Pts',(0.629508251968404,-0.219236411496476,
0.631527555489181));
#24442=CARTESIAN_POINT('Ctrl Pts',(0.64670834881537,-0.204076596372851,
0.614041903462993));
#24443=CARTESIAN_POINT('Ctrl Pts',(0.656687581895314,-0.192197739766234,
0.60329448442429));
#24444=CARTESIAN_POINT('Ctrl Pts',(0.665417486529536,-0.17859,0.593506844649423));
#24445=CARTESIAN_POINT('',(0.888209879025751,-0.22859,0.960664362212974));
#24446=CARTESIAN_POINT('Origin',(0.685838782044607,-0.22859,0.860014630714833));
#24447=CARTESIAN_POINT('Ctrl Pts',(0.950212795795147,-0.178589999999999,
0.899382259516035));
#24448=CARTESIAN_POINT('Ctrl Pts',(0.940291787100225,-0.190965925779192,
0.909863975504277));
#24449=CARTESIAN_POINT('Ctrl Pts',(0.928778132229906,-0.202063936711525,
0.921629874276332));
#24450=CARTESIAN_POINT('Ctrl Pts',(0.90883082946763,-0.217292055674528,
0.941263736526708));
#24451=CARTESIAN_POINT('Ctrl Pts',(0.898853482029647,-0.223500193956903,
0.950823512787988));
#24452=CARTESIAN_POINT('Ctrl Pts',(0.888209879025751,-0.228590000000001,
0.960664362212974));
#24453=CARTESIAN_POINT('Origin',(0.,-0.20359,0.));
#24454=CARTESIAN_POINT('',(1.30486744394591,-0.22859,0.0954660136125388));
#24455=CARTESIAN_POINT('Origin',(0.,-0.22859,0.));
#24456=CARTESIAN_POINT('',(1.29561335303682,-0.17859,0.182150612015699));
#24457=CARTESIAN_POINT('Ctrl Pts',(1.30486744394591,-0.228590000000001,
0.0954660136125391));
#24458=CARTESIAN_POINT('Ctrl Pts',(1.30380973597919,-0.223500193956903,
0.109923186785982));
#24459=CARTESIAN_POINT('Ctrl Pts',(1.30255637630995,-0.217292055674527,
0.123684214131479));
#24460=CARTESIAN_POINT('Ctrl Pts',(1.29964294452704,-0.202063936711524,
0.151521156305556));
#24461=CARTESIAN_POINT('Ctrl Pts',(1.29762264084128,-0.190965925779192,
0.167858812055521));
#24462=CARTESIAN_POINT('Ctrl Pts',(1.29561335303682,-0.178589999999999,
0.182150612015698));
#24463=CARTESIAN_POINT('Origin',(0.,-0.17859,0.));
#24464=CARTESIAN_POINT('Origin',(0.891645,-0.22859,0.));
#24465=CARTESIAN_POINT('',(0.888157443945909,-0.22859,0.0787855366705671));
#24466=CARTESIAN_POINT('Origin',(0.,-0.22859,0.));
#24467=CARTESIAN_POINT('Origin',(1.1,-0.22859,0.));
#24468=CARTESIAN_POINT('Origin',(0.,-0.20359,0.));
#24469=CARTESIAN_POINT('',(0.878903353036818,-0.17859,0.150198874981266));
#24470=CARTESIAN_POINT('Origin',(0.,-0.17859,0.));
#24471=CARTESIAN_POINT('Ctrl Pts',(0.878903353036818,-0.17859,0.150198874981266));
#24472=CARTESIAN_POINT('Ctrl Pts',(0.881112631441229,-0.192197739766234,
0.137271067115392));
#24473=CARTESIAN_POINT('Ctrl Pts',(0.883293351945246,-0.204076596372851,
0.122768082355672));
#24474=CARTESIAN_POINT('Ctrl Pts',(0.886240100215735,-0.219236411496476,
0.0984183794220357));
#24475=CARTESIAN_POINT('Ctrl Pts',(0.887262775645244,-0.224284758603913,
0.0888712242812338));
#24476=CARTESIAN_POINT('Ctrl Pts',(0.888157443945909,-0.22859,0.0787855366705671));
#24477=CARTESIAN_POINT('Origin',(1.308355,-0.17859,0.));
#24478=CARTESIAN_POINT('Origin',(1.1,-0.17859,0.));
#24479=CARTESIAN_POINT('Origin',(1.1,0.,0.));
#24480=CARTESIAN_POINT('Origin',(-0.244773027351946,0.,1.07242070340001));
#24481=CARTESIAN_POINT('',(-0.120823405150736,-0.22859,0.883420913717115));
#24482=CARTESIAN_POINT('',(-0.0491413193775446,-0.17859,0.890289804925809));
#24483=CARTESIAN_POINT('Ctrl Pts',(-0.120823405150736,-0.22859,0.883420913717114));
#24484=CARTESIAN_POINT('Ctrl Pts',(-0.110791504359706,-0.224284758603913,
0.884792953245369));
#24485=CARTESIAN_POINT('Ctrl Pts',(-0.101256149639299,-0.219236411496475,
0.885920360302595));
#24486=CARTESIAN_POINT('Ctrl Pts',(-0.0768612314186785,-0.204076596372851,
0.888465811801873));
#24487=CARTESIAN_POINT('Ctrl Pts',(-0.0622366108032284,-0.192197739766234,
0.889566984227727));
#24488=CARTESIAN_POINT('Ctrl Pts',(-0.0491413193775446,-0.17859,0.890289804925809));
#24489=CARTESIAN_POINT('',(-0.197287840980439,-0.22859,1.29339487931037));
#24490=CARTESIAN_POINT('Origin',(-0.244773027351946,-0.22859,1.07242070340001));
#24491=CARTESIAN_POINT('',(-0.110717377488918,-0.17859,1.30366194557752));
#24492=CARTESIAN_POINT('Ctrl Pts',(-0.110717377488919,-0.178589999999999,
1.30366194557752));
#24493=CARTESIAN_POINT('Ctrl Pts',(-0.125097960784251,-0.190965925779192,
1.30244063166664));
#24494=CARTESIAN_POINT('Ctrl Pts',(-0.14147555725754,-0.202063936711525,
1.30077481170483));
#24495=CARTESIAN_POINT('Ctrl Pts',(-0.169262868734192,-0.217292055674528,
1.29742089529918));
#24496=CARTESIAN_POINT('Ctrl Pts',(-0.182957777157795,-0.223500193956903,
1.2955807139676));
#24497=CARTESIAN_POINT('Ctrl Pts',(-0.197287840980438,-0.228590000000001,
1.29339487931037));
#24498=CARTESIAN_POINT('Origin',(-0.244773027351946,-0.17859,1.07242070340001));
#24499=CARTESIAN_POINT('Origin',(0.,-0.20359,0.));
#24500=CARTESIAN_POINT('',(0.430557068346269,-0.17859,0.780801778252372));
#24501=CARTESIAN_POINT('',(0.492160095813005,-0.22859,0.743511429713312));
#24502=CARTESIAN_POINT('Ctrl Pts',(0.430557068346269,-0.17859,0.780801778252372));
#24503=CARTESIAN_POINT('Ctrl Pts',(0.442041898089724,-0.192197739766234,
0.774468705297715));
#24504=CARTESIAN_POINT('Ctrl Pts',(0.454740445159586,-0.204076596372851,
0.767131198148022));
#24505=CARTESIAN_POINT('Ctrl Pts',(0.475615076997141,-0.219236411496476,
0.754253267259386));
#24506=CARTESIAN_POINT('Ctrl Pts',(0.483716971155137,-0.224284758603913,
0.74910027323947));
#24507=CARTESIAN_POINT('Ctrl Pts',(0.492160095813005,-0.22859,0.743511429713312));
#24508=CARTESIAN_POINT('Origin',(0.,-0.22859,0.));
#24509=CARTESIAN_POINT('Origin',(0.,-0.17859,0.));
#24510=CARTESIAN_POINT('Origin',(1.308355,-0.17859,0.));
#24511=CARTESIAN_POINT('',(0.665390629745762,-0.17859,1.12652035750427));
#24512=CARTESIAN_POINT('Origin',(0.685838782044607,-0.17859,0.860014630714833));
#24513=CARTESIAN_POINT('Origin',(0.,-0.17859,0.));
#24514=CARTESIAN_POINT('Origin',(0.891645,-0.22859,0.));
#24515=CARTESIAN_POINT('',(0.738933209129742,-0.22859,1.07970853403602));
#24516=CARTESIAN_POINT('Origin',(0.685838782044607,-0.22859,0.860014630714833));
#24517=CARTESIAN_POINT('Origin',(0.,-0.22859,0.));
#24518=CARTESIAN_POINT('Origin',(0.,-0.20359,0.));
#24519=CARTESIAN_POINT('Ctrl Pts',(0.738933209129742,-0.228590000000001,
1.07970853403602));
#24520=CARTESIAN_POINT('Ctrl Pts',(0.726970665864657,-0.223500193956903,
1.08789548468573));
#24521=CARTESIAN_POINT('Ctrl Pts',(0.715430404483016,-0.217292055674527,
1.09549542885049));
#24522=CARTESIAN_POINT('Ctrl Pts',(0.69185011171062,-0.202063936711524,
1.11057366572105));
#24523=CARTESIAN_POINT('Ctrl Pts',(0.677817179350845,-0.190965925779192,
1.11918049044176));
#24524=CARTESIAN_POINT('Ctrl Pts',(0.665390629745762,-0.178589999999999,
1.12652035750427));
#24525=CARTESIAN_POINT('Origin',(0.685838782044607,0.,0.860014630714833));
#24526=CARTESIAN_POINT('Origin',(-0.244773027351946,0.,-1.07242070340001));
#24527=CARTESIAN_POINT('',(-0.274443842703457,-0.22859,-0.848358051312746));
#24528=CARTESIAN_POINT('',(-0.342007470572634,-0.17859,-0.823445017045771));
#24529=CARTESIAN_POINT('Ctrl Pts',(-0.274443842703457,-0.22859,-0.848358051312746));
#24530=CARTESIAN_POINT('Ctrl Pts',(-0.284077578642797,-0.224284758603913,
-0.845241537587567));
#24531=CARTESIAN_POINT('Ctrl Pts',(-0.293157799979787,-0.219236411496476,
-0.842120060887678));
#24532=CARTESIAN_POINT('Ctrl Pts',(-0.316241291845841,-0.204076596372851,
-0.833828875110254));
#24533=CARTESIAN_POINT('Ctrl Pts',(-0.329895400534788,-0.192197739766234,
-0.828475612108333));
#24534=CARTESIAN_POINT('Ctrl Pts',(-0.342007470572634,-0.17859,-0.82344501704577));
#24535=CARTESIAN_POINT('',(-0.383432803651626,-0.22859,-1.25090850629007));
#24536=CARTESIAN_POINT('Origin',(-0.244773027351946,-0.22859,-1.07242070340001));
#24537=CARTESIAN_POINT('',(-0.465884809239132,-0.17859,-1.22259729696463));
#24538=CARTESIAN_POINT('Ctrl Pts',(-0.465884809239131,-0.178589999999999,
-1.22259729696463));
#24539=CARTESIAN_POINT('Ctrl Pts',(-0.45239844314147,-0.190965925779192,
-1.22773643240386));
#24540=CARTESIAN_POINT('Ctrl Pts',(-0.436919966394242,-0.202063936711525,
-1.23334155327433));
#24541=CARTESIAN_POINT('Ctrl Pts',(-0.410429254040296,-0.217292055674528,
-1.2423762416108));
#24542=CARTESIAN_POINT('Ctrl Pts',(-0.397292143145055,-0.223500193956903,
-1.24666029359345));
#24543=CARTESIAN_POINT('Ctrl Pts',(-0.383432803651627,-0.228590000000001,
-1.25090850629007));
#24544=CARTESIAN_POINT('Origin',(-0.244773027351946,-0.17859,-1.07242070340001));
#24545=CARTESIAN_POINT('Origin',(0.,-0.20359,0.));
#24546=CARTESIAN_POINT('',(-0.7266957094931,-0.17859,-0.516666383490663));
#24547=CARTESIAN_POINT('',(-0.766018443552043,-0.22859,-0.45634038848551));
#24548=CARTESIAN_POINT('Ctrl Pts',(-0.7266957094931,-0.17859,-0.516666383490663));
#24549=CARTESIAN_POINT('Ctrl Pts',(-0.734295366171442,-0.192197739766234,
-0.505977401048143));
#24550=CARTESIAN_POINT('Ctrl Pts',(-0.74255273671107,-0.204076596372851,
-0.493856842454226));
#24551=CARTESIAN_POINT('Ctrl Pts',(-0.755772605319574,-0.219236411496476,
-0.473197064326185));
#24552=CARTESIAN_POINT('Ctrl Pts',(-0.760836359413957,-0.224284758603913,
-0.465039097006547));
#24553=CARTESIAN_POINT('Ctrl Pts',(-0.766018443552043,-0.22859,-0.45634038848551));
#24554=CARTESIAN_POINT('Origin',(0.,-0.22859,0.));
#24555=CARTESIAN_POINT('Origin',(0.,-0.17859,0.));
#24556=CARTESIAN_POINT('Origin',(1.308355,-0.17859,0.));
#24557=CARTESIAN_POINT('',(-1.08827510730092,-0.17859,-0.726257596761769));
#24558=CARTESIAN_POINT('Origin',(-0.991065754692661,-0.17859,-0.477272113029314));
#24559=CARTESIAN_POINT('Origin',(0.,-0.17859,0.));
#24560=CARTESIAN_POINT('Origin',(0.,-0.20359,0.));
#24561=CARTESIAN_POINT('',(-1.13422379278981,-0.22859,-0.652172671839668));
#24562=CARTESIAN_POINT('Ctrl Pts',(-1.13422379278981,-0.228590000000001,
-0.652172671839668));
#24563=CARTESIAN_POINT('Ctrl Pts',(-1.1269980984869,-0.223500193956903,
-0.66473921249932));
#24564=CARTESIAN_POINT('Ctrl Pts',(-1.11989817444587,-0.217292055674528,
-0.676593657348219));
#24565=CARTESIAN_POINT('Ctrl Pts',(-1.10519526655462,-0.202063936711525,
-0.700409784949027));
#24566=CARTESIAN_POINT('Ctrl Pts',(-1.09628639266483,-0.190965925779192,
-0.714252927236921));
#24567=CARTESIAN_POINT('Ctrl Pts',(-1.08827510730092,-0.178589999999999,
-0.726257596761768));
#24568=CARTESIAN_POINT('Origin',(0.,-0.22859,0.));
#24569=CARTESIAN_POINT('Origin',(0.891645,-0.22859,0.));
#24570=CARTESIAN_POINT('Origin',(-0.991065754692661,-0.22859,-0.477272113029314));
#24571=CARTESIAN_POINT('Origin',(-0.991065754692661,0.,-0.477272113029314));
#24572=CARTESIAN_POINT('Origin',(0.,-0.20359,0.));
#24573=CARTESIAN_POINT('',(0.888209879025751,-0.22859,-0.960664362212974));
#24574=CARTESIAN_POINT('',(0.950212795795148,-0.17859,-0.899382259516035));
#24575=CARTESIAN_POINT('Ctrl Pts',(0.888209879025752,-0.228590000000001,
-0.960664362212974));
#24576=CARTESIAN_POINT('Ctrl Pts',(0.898853482029647,-0.223500193956903,
-0.950823512787987));
#24577=CARTESIAN_POINT('Ctrl Pts',(0.908830829467631,-0.217292055674528,
-0.941263736526708));
#24578=CARTESIAN_POINT('Ctrl Pts',(0.928778132229906,-0.202063936711525,
-0.921629874276332));
#24579=CARTESIAN_POINT('Ctrl Pts',(0.940291787100225,-0.190965925779191,
-0.909863975504277));
#24580=CARTESIAN_POINT('Ctrl Pts',(0.950212795795148,-0.178589999999999,
-0.899382259516035));
#24581=CARTESIAN_POINT('',(1.29561335303682,-0.17859,-0.182150612015699));
#24582=CARTESIAN_POINT('Origin',(0.,-0.17859,0.));
#24583=CARTESIAN_POINT('',(1.30486744394591,-0.22859,-0.0954660136125388));
#24584=CARTESIAN_POINT('Ctrl Pts',(1.29561335303682,-0.178589999999999,
-0.182150612015698));
#24585=CARTESIAN_POINT('Ctrl Pts',(1.29762264084128,-0.190965925779192,
-0.167858812055521));
#24586=CARTESIAN_POINT('Ctrl Pts',(1.29964294452704,-0.202063936711524,
-0.151521156305556));
#24587=CARTESIAN_POINT('Ctrl Pts',(1.30255637630995,-0.217292055674527,
-0.123684214131479));
#24588=CARTESIAN_POINT('Ctrl Pts',(1.30380973597919,-0.223500193956903,
-0.109923186785982));
#24589=CARTESIAN_POINT('Ctrl Pts',(1.30486744394591,-0.228590000000001,
-0.0954660136125391));
#24590=CARTESIAN_POINT('Origin',(0.,-0.22859,0.));
#24591=CARTESIAN_POINT('Origin',(0.891645,-0.22859,0.));
#24592=CARTESIAN_POINT('',(0.615354121677383,-0.22859,-0.64526747241718));
#24593=CARTESIAN_POINT('Origin',(0.685838782044607,-0.22859,-0.860014630714833));
#24594=CARTESIAN_POINT('',(0.888157443945909,-0.22859,-0.0787855366705671));
#24595=CARTESIAN_POINT('Origin',(1.1,-0.22859,0.));
#24596=CARTESIAN_POINT('Origin',(0.,-0.22859,0.));
#24597=CARTESIAN_POINT('Origin',(1.1,0.,0.));
#24598=CARTESIAN_POINT('',(0.878903353036818,-0.17859,-0.150198874981266));
#24599=CARTESIAN_POINT('Origin',(1.1,-0.17859,0.));
#24600=CARTESIAN_POINT('Ctrl Pts',(0.888157443945909,-0.22859,-0.0787855366705672));
#24601=CARTESIAN_POINT('Ctrl Pts',(0.887262775645244,-0.224284758603913,
-0.0888712242812339));
#24602=CARTESIAN_POINT('Ctrl Pts',(0.886240100215735,-0.219236411496476,
-0.0984183794220357));
#24603=CARTESIAN_POINT('Ctrl Pts',(0.883293351945246,-0.204076596372851,
-0.122768082355672));
#24604=CARTESIAN_POINT('Ctrl Pts',(0.881112631441229,-0.192197739766234,
-0.137271067115392));
#24605=CARTESIAN_POINT('Ctrl Pts',(0.878903353036818,-0.17859,-0.150198874981266));
#24606=CARTESIAN_POINT('Origin',(1.308355,-0.17859,0.));
#24607=CARTESIAN_POINT('',(0.665417486529536,-0.17859,-0.593506844649423));
#24608=CARTESIAN_POINT('Origin',(0.685838782044607,-0.17859,-0.860014630714833));
#24609=CARTESIAN_POINT('Origin',(0.,-0.17859,0.));
#24610=CARTESIAN_POINT('Origin',(0.,-0.20359,0.));
#24611=CARTESIAN_POINT('Ctrl Pts',(0.665417486529536,-0.17859,-0.593506844649423));
#24612=CARTESIAN_POINT('Ctrl Pts',(0.656687581895314,-0.192197739766234,
-0.60329448442429));
#24613=CARTESIAN_POINT('Ctrl Pts',(0.64670834881537,-0.204076596372851,
-0.614041903462993));
#24614=CARTESIAN_POINT('Ctrl Pts',(0.629508251968404,-0.219236411496476,
-0.63152755548918));
#24615=CARTESIAN_POINT('Ctrl Pts',(0.622681613212229,-0.224284758603913,
-0.638279669203371));
#24616=CARTESIAN_POINT('Ctrl Pts',(0.615354121677383,-0.22859,-0.64526747241718));
#24617=CARTESIAN_POINT('Origin',(0.685838782044607,0.,-0.860014630714833));
#24618=CARTESIAN_POINT('',(0.,0.,0.));
#24619=CARTESIAN_POINT('Origin',(1.119765,0.495,0.));
#24620=CARTESIAN_POINT('',(-1.119765,0.495,-1.37131662304724E-16));
#24621=CARTESIAN_POINT('Origin',(0.,0.495,0.));
#24622=CARTESIAN_POINT('',(-1.085235,0.495,-1.32902956907268E-16));
#24623=CARTESIAN_POINT('Origin',(0.,0.495,0.));
#24624=CARTESIAN_POINT('Origin',(0.,0.4575,0.));
#24625=CARTESIAN_POINT('',(-1.119765,0.42,-1.37131662304724E-16));
#24626=CARTESIAN_POINT('Origin',(0.,0.42,0.));
#24627=CARTESIAN_POINT('',(-1.119765,0.4575,-1.37131662304724E-16));
#24628=CARTESIAN_POINT('Origin',(1.085235,0.42,0.));
#24629=CARTESIAN_POINT('',(-1.085235,0.42,-1.32902956907268E-16));
#24630=CARTESIAN_POINT('Origin',(0.,0.42,0.));
#24631=CARTESIAN_POINT('Origin',(0.,0.4575,0.));
#24632=CARTESIAN_POINT('',(-1.085235,0.4575,-1.32902956907268E-16));
#24633=CARTESIAN_POINT('Origin',(1.119765,-0.42,0.));
#24634=CARTESIAN_POINT('',(-1.119765,-0.42,-1.37131662304724E-16));
#24635=CARTESIAN_POINT('Origin',(0.,-0.42,0.));
#24636=CARTESIAN_POINT('',(-1.085235,-0.42,-1.32902956907268E-16));
#24637=CARTESIAN_POINT('Origin',(0.,-0.42,0.));
#24638=CARTESIAN_POINT('Origin',(0.,-0.4575,0.));
#24639=CARTESIAN_POINT('',(-1.119765,-0.495,-1.37131662304724E-16));
#24640=CARTESIAN_POINT('Origin',(0.,-0.495,0.));
#24641=CARTESIAN_POINT('',(-1.119765,-0.4575,-1.37131662304724E-16));
#24642=CARTESIAN_POINT('Origin',(1.085235,-0.495,0.));
#24643=CARTESIAN_POINT('',(-1.085235,-0.495,-1.32902956907268E-16));
#24644=CARTESIAN_POINT('Origin',(0.,-0.495,0.));
#24645=CARTESIAN_POINT('Origin',(0.,-0.4575,0.));
#24646=CARTESIAN_POINT('',(-1.085235,-0.4575,-1.32902956907268E-16));
#24647=CARTESIAN_POINT('',(0.,0.,0.));
#24648=CARTESIAN_POINT('',(0.,0.,0.));
#24649=CARTESIAN_POINT('',(0.,0.,0.));
#24650=CARTESIAN_POINT('',(0.,0.,0.));
#24651=CARTESIAN_POINT('',(0.,0.,0.));
#24652=CARTESIAN_POINT('',(0.,0.,0.));
#24653=CARTESIAN_POINT('',(0.,0.,0.));
#24654=CARTESIAN_POINT('',(0.,0.,0.));
#24655=CARTESIAN_POINT('',(0.,0.,0.));
#24656=CARTESIAN_POINT('',(0.,0.,0.));
#24657=CARTESIAN_POINT('',(0.,0.,0.));
#24658=CARTESIAN_POINT('',(0.,0.,0.));
#24659=CARTESIAN_POINT('',(0.,0.,0.));
#24660=CARTESIAN_POINT('',(0.,0.,0.));
#24661=CARTESIAN_POINT('',(0.,0.,0.));
#24662=CARTESIAN_POINT('',(0.,0.,0.));
#24663=CARTESIAN_POINT('',(0.,0.,0.));
#24664=CARTESIAN_POINT('',(0.,0.,0.));
#24665=CARTESIAN_POINT('',(0.,0.,0.));
#24666=CARTESIAN_POINT('',(0.,0.,0.));
#24667=CARTESIAN_POINT('',(0.,0.,0.));
#24668=CARTESIAN_POINT('',(0.,0.,0.));
#24669=CARTESIAN_POINT('',(-1.5,-4.,2.));
#24670=CARTESIAN_POINT('',(-1.5,4.,2.));
#24671=CARTESIAN_POINT('',(1.5,-4.,2.));
#24672=CARTESIAN_POINT('',(1.5,4.,2.));
#24673=CARTESIAN_POINT('',(0.,0.,6.));
#24674=CARTESIAN_POINT('',(-1.3,1.30814754519511,7.30814754519511));
#24675=CARTESIAN_POINT('',(-1.3,-1.30814754519511,7.30814754519511));
#24676=CARTESIAN_POINT('',(-1.3,-1.30814754519511,4.69185245480489));
#24677=CARTESIAN_POINT('',(-1.3,1.30814754519511,4.69185245480489));
#24678=CARTESIAN_POINT('',(1.3,1.30814754519511,7.30814754519511));
#24679=CARTESIAN_POINT('',(1.3,-1.30814754519511,7.30814754519511));
#24680=CARTESIAN_POINT('',(1.3,-1.30814754519511,4.69185245480489));
#24681=CARTESIAN_POINT('',(1.3,1.30814754519511,4.69185245480489));
#24682=CARTESIAN_POINT('',(43.5,-4.,2.));
#24683=CARTESIAN_POINT('',(43.5,4.,2.));
#24684=CARTESIAN_POINT('',(46.5,-4.,2.));
#24685=CARTESIAN_POINT('',(46.5,4.,2.));
#24686=CARTESIAN_POINT('',(45.,0.,6.));
#24687=CARTESIAN_POINT('',(43.7,1.30814754519511,7.30814754519511));
#24688=CARTESIAN_POINT('',(43.7,-1.30814754519511,7.30814754519511));
#24689=CARTESIAN_POINT('',(43.7,-1.30814754519511,4.69185245480489));
#24690=CARTESIAN_POINT('',(43.7,1.30814754519511,4.69185245480489));
#24691=CARTESIAN_POINT('',(46.3,1.30814754519511,7.30814754519511));
#24692=CARTESIAN_POINT('',(46.3,-1.30814754519511,7.30814754519511));
#24693=CARTESIAN_POINT('',(46.3,-1.30814754519511,4.69185245480489));
#24694=CARTESIAN_POINT('',(46.3,1.30814754519511,4.69185245480489));
#24695=CARTESIAN_POINT('',(0.,-7.7,3.));
#24696=CARTESIAN_POINT('',(0.,6.7,3.));
#24697=CARTESIAN_POINT('',(0.,0.,0.));
#24698=CARTESIAN_POINT('',(0.,0.,0.));
#24699=CARTESIAN_POINT('',(0.,0.,0.));
#24700=CARTESIAN_POINT('',(0.,0.,0.));
#24701=CARTESIAN_POINT('',(0.,0.,0.));
#24702=CARTESIAN_POINT('',(0.,0.,0.));
#24703=CARTESIAN_POINT('',(0.,0.,0.));
#24704=CARTESIAN_POINT('',(0.,0.,0.));
#24705=CARTESIAN_POINT('',(0.,0.,0.));
#24706=CARTESIAN_POINT('',(0.,0.,0.));
#24707=CARTESIAN_POINT('',(0.,0.,0.));
#24708=CARTESIAN_POINT('',(0.,0.,0.));
#24709=CARTESIAN_POINT('',(0.,0.,0.));
#24710=CARTESIAN_POINT('',(0.,0.,0.));
#24711=CARTESIAN_POINT('',(0.,0.,0.));
#24712=CARTESIAN_POINT('',(0.,0.,0.));
#24713=CARTESIAN_POINT('',(0.,0.,0.));
#24714=CARTESIAN_POINT('',(0.,0.,0.));
#24715=CARTESIAN_POINT('',(0.,0.,0.));
#24716=CARTESIAN_POINT('',(0.,0.,0.));
#24717=CARTESIAN_POINT('',(0.,0.,0.));
#24718=CARTESIAN_POINT('',(0.,0.,0.));
#24719=CARTESIAN_POINT('',(0.,0.,0.));
#24720=CARTESIAN_POINT('',(0.,0.,0.));
#24721=CARTESIAN_POINT('',(0.,0.,0.));
#24722=CARTESIAN_POINT('',(0.,0.,0.));
#24723=CARTESIAN_POINT('',(19.3649167310371,-5.,8.));
#24724=CARTESIAN_POINT('',(19.3649167310371,7.5,8.));
#24725=CARTESIAN_POINT('',(0.,0.,0.));
#24726=CARTESIAN_POINT('',(0.,0.,0.));
#24727=CARTESIAN_POINT('Origin',(44.5,0.,6.));
#24728=CARTESIAN_POINT('',(44.5,-9.79717439317882E-17,6.8));
#24729=CARTESIAN_POINT('Origin',(44.5,0.,6.));
#24730=CARTESIAN_POINT('',(44.5,-7.34788079488412E-17,6.6));
#24731=CARTESIAN_POINT('Origin',(44.5,0.,6.));
#24732=CARTESIAN_POINT('Origin',(44.,0.,6.));
#24733=CARTESIAN_POINT('',(44.,-9.79717439317882E-17,6.8));
#24734=CARTESIAN_POINT('Origin',(44.,0.,6.));
#24735=CARTESIAN_POINT('',(44.,7.34788079488412E-17,6.6));
#24736=CARTESIAN_POINT('Origin',(44.,0.,6.));
#24737=CARTESIAN_POINT('Origin',(44.,0.,6.));
#24738=CARTESIAN_POINT('',(44.,-9.79717439317882E-17,6.8));
#24739=CARTESIAN_POINT('Origin',(-3.5,0.,6.));
#24740=CARTESIAN_POINT('',(1.,-7.34788079488412E-17,6.6));
#24741=CARTESIAN_POINT('',(-3.5,-7.34788079488412E-17,6.6));
#24742=CARTESIAN_POINT('Origin',(1.,0.,6.));
#24743=CARTESIAN_POINT('Origin',(1.,0.,6.));
#24744=CARTESIAN_POINT('',(1.,-9.79717439317882E-17,6.8));
#24745=CARTESIAN_POINT('Origin',(1.,0.,6.));
#24746=CARTESIAN_POINT('Origin',(0.5,0.,6.));
#24747=CARTESIAN_POINT('',(0.5,-9.79717439317882E-17,6.8));
#24748=CARTESIAN_POINT('Origin',(0.5,0.,6.));
#24749=CARTESIAN_POINT('',(0.5,7.34788079488412E-17,6.6));
#24750=CARTESIAN_POINT('Origin',(0.5,0.,6.));
#24751=CARTESIAN_POINT('Origin',(0.5,0.,6.));
#24752=CARTESIAN_POINT('',(0.5,-9.79717439317882E-17,6.8));
#24753=CARTESIAN_POINT('Origin',(-3.5,0.,6.));
#24754=CARTESIAN_POINT('',(-3.5,-7.34788079488412E-17,6.6));
#24755=CARTESIAN_POINT('',(-3.5,-7.34788079488412E-17,6.6));
#24756=CARTESIAN_POINT('Origin',(-3.5,0.,6.));
#24757=CARTESIAN_POINT('Origin',(-3.5,0.,6.));
#24758=CARTESIAN_POINT('',(47.,-7.34788079488412E-17,6.6));
#24759=CARTESIAN_POINT('Origin',(47.,0.,6.));
#24760=CARTESIAN_POINT('',(-3.5,-7.34788079488412E-17,6.6));
#24761=CARTESIAN_POINT('Origin',(47.,0.,6.));
#24762=CARTESIAN_POINT('Origin',(-3.5,0.,6.));
#24763=CARTESIAN_POINT('',(0.,0.,0.));
#24764=CARTESIAN_POINT('Origin',(-1.3,0.,6.));
#24765=CARTESIAN_POINT('',(-0.5,-7.40911313484149E-17,6.605));
#24766=CARTESIAN_POINT('Origin',(-0.5,0.,6.));
#24767=CARTESIAN_POINT('',(-1.3,-7.40911313484149E-17,6.605));
#24768=CARTESIAN_POINT('',(-1.3,-7.40911313484149E-17,6.605));
#24769=CARTESIAN_POINT('Origin',(-1.3,0.,6.));
#24770=CARTESIAN_POINT('Origin',(-1.3,0.,6.));
#24771=CARTESIAN_POINT('',(-0.5,-9.79717439317882E-17,6.8));
#24772=CARTESIAN_POINT('Origin',(-0.5,0.,6.));
#24773=CARTESIAN_POINT('',(-1.3,-9.79717439317882E-17,6.8));
#24774=CARTESIAN_POINT('',(-1.3,-9.79717439317882E-17,6.8));
#24775=CARTESIAN_POINT('Origin',(-1.3,0.,6.));
#24776=CARTESIAN_POINT('Origin',(-0.5,0.,6.));
#24777=CARTESIAN_POINT('Origin',(-1.3,0.,6.));
#24778=CARTESIAN_POINT('',(0.,0.,0.));
#24779=CARTESIAN_POINT('Origin',(45.5,0.,6.));
#24780=CARTESIAN_POINT('',(46.3,-7.40911313484149E-17,6.605));
#24781=CARTESIAN_POINT('Origin',(46.3,0.,6.));
#24782=CARTESIAN_POINT('',(45.5,-7.40911313484149E-17,6.605));
#24783=CARTESIAN_POINT('',(45.5,-7.40911313484149E-17,6.605));
#24784=CARTESIAN_POINT('Origin',(45.5,0.,6.));
#24785=CARTESIAN_POINT('Origin',(45.5,0.,6.));
#24786=CARTESIAN_POINT('',(46.3,-9.79717439317882E-17,6.8));
#24787=CARTESIAN_POINT('Origin',(46.3,0.,6.));
#24788=CARTESIAN_POINT('',(45.5,-9.79717439317882E-17,6.8));
#24789=CARTESIAN_POINT('',(45.5,-9.79717439317882E-17,6.8));
#24790=CARTESIAN_POINT('Origin',(45.5,0.,6.));
#24791=CARTESIAN_POINT('Origin',(46.3,0.,6.));
#24792=CARTESIAN_POINT('Origin',(45.5,0.,6.));
#24793=CARTESIAN_POINT('',(0.,0.,0.));
#24794=CARTESIAN_POINT('Origin',(-1.5,0.,6.));
#24795=CARTESIAN_POINT('',(-1.3,-7.34788079488412E-17,6.6));
#24796=CARTESIAN_POINT('Origin',(-1.3,0.,6.));
#24797=CARTESIAN_POINT('',(-1.5,-7.34788079488412E-17,6.6));
#24798=CARTESIAN_POINT('',(-1.5,-7.34788079488412E-17,6.6));
#24799=CARTESIAN_POINT('Origin',(-1.5,0.,6.));
#24800=CARTESIAN_POINT('Origin',(-1.5,0.,6.));
#24801=CARTESIAN_POINT('',(-1.3,-1.10218211923262E-16,6.9));
#24802=CARTESIAN_POINT('Origin',(-1.3,0.,6.));
#24803=CARTESIAN_POINT('',(-1.5,-1.10218211923262E-16,6.9));
#24804=CARTESIAN_POINT('',(-1.5,-1.10218211923262E-16,6.9));
#24805=CARTESIAN_POINT('Origin',(-1.5,0.,6.));
#24806=CARTESIAN_POINT('Origin',(-1.3,0.,6.));
#24807=CARTESIAN_POINT('Origin',(-1.5,0.,6.));
#24808=CARTESIAN_POINT('',(0.,0.,0.));
#24809=CARTESIAN_POINT('Origin',(46.3,0.,6.));
#24810=CARTESIAN_POINT('',(46.5,-7.34788079488412E-17,6.6));
#24811=CARTESIAN_POINT('Origin',(46.5,0.,6.));
#24812=CARTESIAN_POINT('',(46.3,-7.34788079488412E-17,6.6));
#24813=CARTESIAN_POINT('',(46.3,-7.34788079488412E-17,6.6));
#24814=CARTESIAN_POINT('Origin',(46.3,0.,6.));
#24815=CARTESIAN_POINT('Origin',(46.3,0.,6.));
#24816=CARTESIAN_POINT('',(46.5,-1.10218211923262E-16,6.9));
#24817=CARTESIAN_POINT('Origin',(46.5,0.,6.));
#24818=CARTESIAN_POINT('',(46.3,-1.10218211923262E-16,6.9));
#24819=CARTESIAN_POINT('',(46.3,-1.10218211923262E-16,6.9));
#24820=CARTESIAN_POINT('Origin',(46.3,0.,6.));
#24821=CARTESIAN_POINT('Origin',(46.5,0.,6.));
#24822=CARTESIAN_POINT('Origin',(46.3,0.,6.));
#24823=CARTESIAN_POINT('',(0.,0.,0.));
#24824=CARTESIAN_POINT('Origin',(-5.5,0.,7.5));
#24825=CARTESIAN_POINT('',(-3.5,-4.89858719658942E-17,7.9));
#24826=CARTESIAN_POINT('Origin',(-3.5,0.,7.5));
#24827=CARTESIAN_POINT('',(-5.5,-4.89858719658942E-17,7.9));
#24828=CARTESIAN_POINT('',(-5.5,-4.89858719658942E-17,7.9));
#24829=CARTESIAN_POINT('Origin',(-5.5,0.,7.5));
#24830=CARTESIAN_POINT('Origin',(-5.5,0.,7.5));
#24831=CARTESIAN_POINT('Origin',(-3.5,0.,6.));
#24832=CARTESIAN_POINT('',(-2.7,-7.34788079488412E-17,6.6));
#24833=CARTESIAN_POINT('Origin',(-2.7,0.,6.));
#24834=CARTESIAN_POINT('',(-3.5,-7.34788079488412E-17,6.6));
#24835=CARTESIAN_POINT('',(-3.5,-7.34788079488412E-17,6.6));
#24836=CARTESIAN_POINT('Origin',(-3.5,0.,6.));
#24837=CARTESIAN_POINT('Origin',(-3.5,0.,6.));
#24838=CARTESIAN_POINT('',(-2.7,-2.44929359829471E-16,8.));
#24839=CARTESIAN_POINT('Origin',(-2.7,0.,6.));
#24840=CARTESIAN_POINT('',(-3.5,-2.44929359829471E-16,8.));
#24841=CARTESIAN_POINT('',(-3.5,-2.44929359829471E-16,8.));
#24842=CARTESIAN_POINT('Origin',(-3.5,0.,6.));
#24843=CARTESIAN_POINT('Origin',(-2.7,0.,6.));
#24844=CARTESIAN_POINT('Origin',(-3.5,0.,6.));
#24845=CARTESIAN_POINT('',(0.,0.,0.));
#24846=CARTESIAN_POINT('',(0.,0.,0.));
#24847=CARTESIAN_POINT('',(0.,0.,0.));
#24848=CARTESIAN_POINT('',(0.,0.,0.));
#24849=CARTESIAN_POINT('',(0.,0.,0.));
#24850=CARTESIAN_POINT('',(0.,0.,0.));
#24851=CARTESIAN_POINT('',(0.,0.,0.));
#24852=CARTESIAN_POINT('',(2.2303625918567E-46,0.,5.6460033311814));
#24853=CARTESIAN_POINT('',(-1.9167572559102,6.74700668366753E-80,2.63223580348951E-15));
#24854=CARTESIAN_POINT('',(-1.91675725591021,-1.46371787188162E-80,5.64600333118141));
#24855=CARTESIAN_POINT('',(0.445943139941388,1.30379860562162E-17,0.0333293549940219));
#24856=CARTESIAN_POINT('',(-1.93242027307935,8.67328754960536E-17,5.79043053615549));
#24857=CARTESIAN_POINT('',(5.17509650795843E-16,-3.84799824028755,10.6035757344421));
#24858=CARTESIAN_POINT('Origin',(0.,0.,0.));
#24859=UNCERTAINTY_MEASURE_WITH_UNIT(LENGTH_MEASURE(0.001),#25101,
'DISTANCE_ACCURACY_VALUE',
'Maximum model space distance between geometric entities at asserted c
onnectivities');
#24860=UNCERTAINTY_MEASURE_WITH_UNIT(LENGTH_MEASURE(0.001),#25101,
'DISTANCE_ACCURACY_VALUE',
'Maximum model space distance between geometric entities at asserted c
onnectivities');
#24861=UNCERTAINTY_MEASURE_WITH_UNIT(LENGTH_MEASURE(0.001),#25101,
'DISTANCE_ACCURACY_VALUE',
'Maximum model space distance between geometric entities at asserted c
onnectivities');
#24862=UNCERTAINTY_MEASURE_WITH_UNIT(LENGTH_MEASURE(0.001),#25101,
'DISTANCE_ACCURACY_VALUE',
'Maximum model space distance between geometric entities at asserted c
onnectivities');
#24863=UNCERTAINTY_MEASURE_WITH_UNIT(LENGTH_MEASURE(0.001),#25101,
'DISTANCE_ACCURACY_VALUE',
'Maximum model space distance between geometric entities at asserted c
onnectivities');
#24864=UNCERTAINTY_MEASURE_WITH_UNIT(LENGTH_MEASURE(0.001),#25101,
'DISTANCE_ACCURACY_VALUE',
'Maximum model space distance between geometric entities at asserted c
onnectivities');
#24865=UNCERTAINTY_MEASURE_WITH_UNIT(LENGTH_MEASURE(0.001),#25101,
'DISTANCE_ACCURACY_VALUE',
'Maximum model space distance between geometric entities at asserted c
onnectivities');
#24866=UNCERTAINTY_MEASURE_WITH_UNIT(LENGTH_MEASURE(0.001),#25101,
'DISTANCE_ACCURACY_VALUE',
'Maximum model space distance between geometric entities at asserted c
onnectivities');
#24867=UNCERTAINTY_MEASURE_WITH_UNIT(LENGTH_MEASURE(0.001),#25101,
'DISTANCE_ACCURACY_VALUE',
'Maximum model space distance between geometric entities at asserted c
onnectivities');
#24868=UNCERTAINTY_MEASURE_WITH_UNIT(LENGTH_MEASURE(0.001),#25101,
'DISTANCE_ACCURACY_VALUE',
'Maximum model space distance between geometric entities at asserted c
onnectivities');
#24869=UNCERTAINTY_MEASURE_WITH_UNIT(LENGTH_MEASURE(0.001),#25101,
'DISTANCE_ACCURACY_VALUE',
'Maximum model space distance between geometric entities at asserted c
onnectivities');
#24870=UNCERTAINTY_MEASURE_WITH_UNIT(LENGTH_MEASURE(0.001),#25101,
'DISTANCE_ACCURACY_VALUE',
'Maximum model space distance between geometric entities at asserted c
onnectivities');
#24871=UNCERTAINTY_MEASURE_WITH_UNIT(LENGTH_MEASURE(0.001),#25101,
'DISTANCE_ACCURACY_VALUE',
'Maximum model space distance between geometric entities at asserted c
onnectivities');
#24872=UNCERTAINTY_MEASURE_WITH_UNIT(LENGTH_MEASURE(0.001),#25101,
'DISTANCE_ACCURACY_VALUE',
'Maximum model space distance between geometric entities at asserted c
onnectivities');
#24873=UNCERTAINTY_MEASURE_WITH_UNIT(LENGTH_MEASURE(0.001),#25101,
'DISTANCE_ACCURACY_VALUE',
'Maximum model space distance between geometric entities at asserted c
onnectivities');
#24874=UNCERTAINTY_MEASURE_WITH_UNIT(LENGTH_MEASURE(0.001),#25101,
'DISTANCE_ACCURACY_VALUE',
'Maximum model space distance between geometric entities at asserted c
onnectivities');
#24875=UNCERTAINTY_MEASURE_WITH_UNIT(LENGTH_MEASURE(0.001),#25101,
'DISTANCE_ACCURACY_VALUE',
'Maximum model space distance between geometric entities at asserted c
onnectivities');
#24876=UNCERTAINTY_MEASURE_WITH_UNIT(LENGTH_MEASURE(0.001),#25101,
'DISTANCE_ACCURACY_VALUE',
'Maximum model space distance between geometric entities at asserted c
onnectivities');
#24877=UNCERTAINTY_MEASURE_WITH_UNIT(LENGTH_MEASURE(0.001),#25101,
'DISTANCE_ACCURACY_VALUE',
'Maximum model space distance between geometric entities at asserted c
onnectivities');
#24878=UNCERTAINTY_MEASURE_WITH_UNIT(LENGTH_MEASURE(0.001),#25101,
'DISTANCE_ACCURACY_VALUE',
'Maximum model space distance between geometric entities at asserted c
onnectivities');
#24879=UNCERTAINTY_MEASURE_WITH_UNIT(LENGTH_MEASURE(0.001),#25101,
'DISTANCE_ACCURACY_VALUE',
'Maximum model space distance between geometric entities at asserted c
onnectivities');
#24880=UNCERTAINTY_MEASURE_WITH_UNIT(LENGTH_MEASURE(0.001),#25101,
'DISTANCE_ACCURACY_VALUE',
'Maximum model space distance between geometric entities at asserted c
onnectivities');
#24881=UNCERTAINTY_MEASURE_WITH_UNIT(LENGTH_MEASURE(0.001),#25101,
'DISTANCE_ACCURACY_VALUE',
'Maximum model space distance between geometric entities at asserted c
onnectivities');
#24882=UNCERTAINTY_MEASURE_WITH_UNIT(LENGTH_MEASURE(0.001),#25101,
'DISTANCE_ACCURACY_VALUE',
'Maximum model space distance between geometric entities at asserted c
onnectivities');
#24883=UNCERTAINTY_MEASURE_WITH_UNIT(LENGTH_MEASURE(0.001),#25101,
'DISTANCE_ACCURACY_VALUE',
'Maximum model space distance between geometric entities at asserted c
onnectivities');
#24884=UNCERTAINTY_MEASURE_WITH_UNIT(LENGTH_MEASURE(0.001),#25101,
'DISTANCE_ACCURACY_VALUE',
'Maximum model space distance between geometric entities at asserted c
onnectivities');
#24885=UNCERTAINTY_MEASURE_WITH_UNIT(LENGTH_MEASURE(0.001),#25101,
'DISTANCE_ACCURACY_VALUE',
'Maximum model space distance between geometric entities at asserted c
onnectivities');
#24886=UNCERTAINTY_MEASURE_WITH_UNIT(LENGTH_MEASURE(0.001),#25101,
'DISTANCE_ACCURACY_VALUE',
'Maximum model space distance between geometric entities at asserted c
onnectivities');
#24887=UNCERTAINTY_MEASURE_WITH_UNIT(LENGTH_MEASURE(0.001),#25101,
'DISTANCE_ACCURACY_VALUE',
'Maximum model space distance between geometric entities at asserted c
onnectivities');
#24888=UNCERTAINTY_MEASURE_WITH_UNIT(LENGTH_MEASURE(0.001),#25101,
'DISTANCE_ACCURACY_VALUE',
'Maximum model space distance between geometric entities at asserted c
onnectivities');
#24889=UNCERTAINTY_MEASURE_WITH_UNIT(LENGTH_MEASURE(0.001),#25101,
'DISTANCE_ACCURACY_VALUE',
'Maximum model space distance between geometric entities at asserted c
onnectivities');
#24890=UNCERTAINTY_MEASURE_WITH_UNIT(LENGTH_MEASURE(0.001),#25101,
'DISTANCE_ACCURACY_VALUE',
'Maximum model space distance between geometric entities at asserted c
onnectivities');
#24891=UNCERTAINTY_MEASURE_WITH_UNIT(LENGTH_MEASURE(0.001),#25101,
'DISTANCE_ACCURACY_VALUE',
'Maximum model space distance between geometric entities at asserted c
onnectivities');
#24892=UNCERTAINTY_MEASURE_WITH_UNIT(LENGTH_MEASURE(0.001),#25101,
'DISTANCE_ACCURACY_VALUE',
'Maximum model space distance between geometric entities at asserted c
onnectivities');
#24893=UNCERTAINTY_MEASURE_WITH_UNIT(LENGTH_MEASURE(0.001),#25101,
'DISTANCE_ACCURACY_VALUE',
'Maximum model space distance between geometric entities at asserted c
onnectivities');
#24894=UNCERTAINTY_MEASURE_WITH_UNIT(LENGTH_MEASURE(0.001),#25101,
'DISTANCE_ACCURACY_VALUE',
'Maximum model space distance between geometric entities at asserted c
onnectivities');
#24895=UNCERTAINTY_MEASURE_WITH_UNIT(LENGTH_MEASURE(0.001),#25101,
'DISTANCE_ACCURACY_VALUE',
'Maximum model space distance between geometric entities at asserted c
onnectivities');
#24896=UNCERTAINTY_MEASURE_WITH_UNIT(LENGTH_MEASURE(0.001),#25101,
'DISTANCE_ACCURACY_VALUE',
'Maximum model space distance between geometric entities at asserted c
onnectivities');
#24897=UNCERTAINTY_MEASURE_WITH_UNIT(LENGTH_MEASURE(0.001),#25101,
'DISTANCE_ACCURACY_VALUE',
'Maximum model space distance between geometric entities at asserted c
onnectivities');
#24898=UNCERTAINTY_MEASURE_WITH_UNIT(LENGTH_MEASURE(0.001),#25101,
'DISTANCE_ACCURACY_VALUE',
'Maximum model space distance between geometric entities at asserted c
onnectivities');
#24899=UNCERTAINTY_MEASURE_WITH_UNIT(LENGTH_MEASURE(0.001),#25101,
'DISTANCE_ACCURACY_VALUE',
'Maximum model space distance between geometric entities at asserted c
onnectivities');
#24900=UNCERTAINTY_MEASURE_WITH_UNIT(LENGTH_MEASURE(0.001),#25101,
'DISTANCE_ACCURACY_VALUE',
'Maximum model space distance between geometric entities at asserted c
onnectivities');
#24901=UNCERTAINTY_MEASURE_WITH_UNIT(LENGTH_MEASURE(0.001),#25101,
'DISTANCE_ACCURACY_VALUE',
'Maximum model space distance between geometric entities at asserted c
onnectivities');
#24902=UNCERTAINTY_MEASURE_WITH_UNIT(LENGTH_MEASURE(0.001),#25101,
'DISTANCE_ACCURACY_VALUE',
'Maximum model space distance between geometric entities at asserted c
onnectivities');
#24903=UNCERTAINTY_MEASURE_WITH_UNIT(LENGTH_MEASURE(0.001),#25101,
'DISTANCE_ACCURACY_VALUE',
'Maximum model space distance between geometric entities at asserted c
onnectivities');
#24904=UNCERTAINTY_MEASURE_WITH_UNIT(LENGTH_MEASURE(0.001),#25101,
'DISTANCE_ACCURACY_VALUE',
'Maximum model space distance between geometric entities at asserted c
onnectivities');
#24905=UNCERTAINTY_MEASURE_WITH_UNIT(LENGTH_MEASURE(0.001),#25101,
'DISTANCE_ACCURACY_VALUE',
'Maximum model space distance between geometric entities at asserted c
onnectivities');
#24906=UNCERTAINTY_MEASURE_WITH_UNIT(LENGTH_MEASURE(0.001),#25101,
'DISTANCE_ACCURACY_VALUE',
'Maximum model space distance between geometric entities at asserted c
onnectivities');
#24907=UNCERTAINTY_MEASURE_WITH_UNIT(LENGTH_MEASURE(0.001),#25101,
'DISTANCE_ACCURACY_VALUE',
'Maximum model space distance between geometric entities at asserted c
onnectivities');
#24908=UNCERTAINTY_MEASURE_WITH_UNIT(LENGTH_MEASURE(0.001),#25101,
'DISTANCE_ACCURACY_VALUE',
'Maximum model space distance between geometric entities at asserted c
onnectivities');
#24909=UNCERTAINTY_MEASURE_WITH_UNIT(LENGTH_MEASURE(0.001),#25101,
'DISTANCE_ACCURACY_VALUE',
'Maximum model space distance between geometric entities at asserted c
onnectivities');
#24910=UNCERTAINTY_MEASURE_WITH_UNIT(LENGTH_MEASURE(0.001),#25101,
'DISTANCE_ACCURACY_VALUE',
'Maximum model space distance between geometric entities at asserted c
onnectivities');
#24911=UNCERTAINTY_MEASURE_WITH_UNIT(LENGTH_MEASURE(0.001),#25101,
'DISTANCE_ACCURACY_VALUE',
'Maximum model space distance between geometric entities at asserted c
onnectivities');
#24912=UNCERTAINTY_MEASURE_WITH_UNIT(LENGTH_MEASURE(0.001),#25101,
'DISTANCE_ACCURACY_VALUE',
'Maximum model space distance between geometric entities at asserted c
onnectivities');
#24913=UNCERTAINTY_MEASURE_WITH_UNIT(LENGTH_MEASURE(0.001),#25101,
'DISTANCE_ACCURACY_VALUE',
'Maximum model space distance between geometric entities at asserted c
onnectivities');
#24914=UNCERTAINTY_MEASURE_WITH_UNIT(LENGTH_MEASURE(0.001),#25101,
'DISTANCE_ACCURACY_VALUE',
'Maximum model space distance between geometric entities at asserted c
onnectivities');
#24915=UNCERTAINTY_MEASURE_WITH_UNIT(LENGTH_MEASURE(0.001),#25101,
'DISTANCE_ACCURACY_VALUE',
'Maximum model space distance between geometric entities at asserted c
onnectivities');
#24916=UNCERTAINTY_MEASURE_WITH_UNIT(LENGTH_MEASURE(0.001),#25101,
'DISTANCE_ACCURACY_VALUE',
'Maximum model space distance between geometric entities at asserted c
onnectivities');
#24917=UNCERTAINTY_MEASURE_WITH_UNIT(LENGTH_MEASURE(0.001),#25101,
'DISTANCE_ACCURACY_VALUE',
'Maximum model space distance between geometric entities at asserted c
onnectivities');
#24918=UNCERTAINTY_MEASURE_WITH_UNIT(LENGTH_MEASURE(0.001),#25101,
'DISTANCE_ACCURACY_VALUE',
'Maximum model space distance between geometric entities at asserted c
onnectivities');
#24919=UNCERTAINTY_MEASURE_WITH_UNIT(LENGTH_MEASURE(0.001),#25101,
'DISTANCE_ACCURACY_VALUE',
'Maximum model space distance between geometric entities at asserted c
onnectivities');
#24920=UNCERTAINTY_MEASURE_WITH_UNIT(LENGTH_MEASURE(0.001),#25101,
'DISTANCE_ACCURACY_VALUE',
'Maximum model space distance between geometric entities at asserted c
onnectivities');
#24921=UNCERTAINTY_MEASURE_WITH_UNIT(LENGTH_MEASURE(0.001),#25101,
'DISTANCE_ACCURACY_VALUE',
'Maximum model space distance between geometric entities at asserted c
onnectivities');
#24922=UNCERTAINTY_MEASURE_WITH_UNIT(LENGTH_MEASURE(0.001),#25101,
'DISTANCE_ACCURACY_VALUE',
'Maximum model space distance between geometric entities at asserted c
onnectivities');
#24923=UNCERTAINTY_MEASURE_WITH_UNIT(LENGTH_MEASURE(0.001),#25101,
'DISTANCE_ACCURACY_VALUE',
'Maximum model space distance between geometric entities at asserted c
onnectivities');
#24924=UNCERTAINTY_MEASURE_WITH_UNIT(LENGTH_MEASURE(0.001),#25101,
'DISTANCE_ACCURACY_VALUE',
'Maximum model space distance between geometric entities at asserted c
onnectivities');
#24925=UNCERTAINTY_MEASURE_WITH_UNIT(LENGTH_MEASURE(0.001),#25101,
'DISTANCE_ACCURACY_VALUE',
'Maximum model space distance between geometric entities at asserted c
onnectivities');
#24926=UNCERTAINTY_MEASURE_WITH_UNIT(LENGTH_MEASURE(0.001),#25101,
'DISTANCE_ACCURACY_VALUE',
'Maximum model space distance between geometric entities at asserted c
onnectivities');
#24927=UNCERTAINTY_MEASURE_WITH_UNIT(LENGTH_MEASURE(0.001),#25101,
'DISTANCE_ACCURACY_VALUE',
'Maximum model space distance between geometric entities at asserted c
onnectivities');
#24928=UNCERTAINTY_MEASURE_WITH_UNIT(LENGTH_MEASURE(0.001),#25101,
'DISTANCE_ACCURACY_VALUE',
'Maximum model space distance between geometric entities at asserted c
onnectivities');
#24929=UNCERTAINTY_MEASURE_WITH_UNIT(LENGTH_MEASURE(0.001),#25101,
'DISTANCE_ACCURACY_VALUE',
'Maximum model space distance between geometric entities at asserted c
onnectivities');
#24930=UNCERTAINTY_MEASURE_WITH_UNIT(LENGTH_MEASURE(0.001),#25101,
'DISTANCE_ACCURACY_VALUE',
'Maximum model space distance between geometric entities at asserted c
onnectivities');
#24931=UNCERTAINTY_MEASURE_WITH_UNIT(LENGTH_MEASURE(0.001),#25101,
'DISTANCE_ACCURACY_VALUE',
'Maximum model space distance between geometric entities at asserted c
onnectivities');
#24932=UNCERTAINTY_MEASURE_WITH_UNIT(LENGTH_MEASURE(0.001),#25101,
'DISTANCE_ACCURACY_VALUE',
'Maximum model space distance between geometric entities at asserted c
onnectivities');
#24933=UNCERTAINTY_MEASURE_WITH_UNIT(LENGTH_MEASURE(0.001),#25101,
'DISTANCE_ACCURACY_VALUE',
'Maximum model space distance between geometric entities at asserted c
onnectivities');
#24934=UNCERTAINTY_MEASURE_WITH_UNIT(LENGTH_MEASURE(0.001),#25101,
'DISTANCE_ACCURACY_VALUE',
'Maximum model space distance between geometric entities at asserted c
onnectivities');
#24935=UNCERTAINTY_MEASURE_WITH_UNIT(LENGTH_MEASURE(0.001),#25101,
'DISTANCE_ACCURACY_VALUE',
'Maximum model space distance between geometric entities at asserted c
onnectivities');
#24936=UNCERTAINTY_MEASURE_WITH_UNIT(LENGTH_MEASURE(0.001),#25101,
'DISTANCE_ACCURACY_VALUE',
'Maximum model space distance between geometric entities at asserted c
onnectivities');
#24937=UNCERTAINTY_MEASURE_WITH_UNIT(LENGTH_MEASURE(0.001),#25101,
'DISTANCE_ACCURACY_VALUE',
'Maximum model space distance between geometric entities at asserted c
onnectivities');
#24938=UNCERTAINTY_MEASURE_WITH_UNIT(LENGTH_MEASURE(0.001),#25101,
'DISTANCE_ACCURACY_VALUE',
'Maximum model space distance between geometric entities at asserted c
onnectivities');
#24939=UNCERTAINTY_MEASURE_WITH_UNIT(LENGTH_MEASURE(0.001),#25101,
'DISTANCE_ACCURACY_VALUE',
'Maximum model space distance between geometric entities at asserted c
onnectivities');
#24940=UNCERTAINTY_MEASURE_WITH_UNIT(LENGTH_MEASURE(0.001),#25101,
'DISTANCE_ACCURACY_VALUE',
'Maximum model space distance between geometric entities at asserted c
onnectivities');
#24941=UNCERTAINTY_MEASURE_WITH_UNIT(LENGTH_MEASURE(0.001),#25101,
'DISTANCE_ACCURACY_VALUE',
'Maximum model space distance between geometric entities at asserted c
onnectivities');
#24942=UNCERTAINTY_MEASURE_WITH_UNIT(LENGTH_MEASURE(0.001),#25101,
'DISTANCE_ACCURACY_VALUE',
'Maximum model space distance between geometric entities at asserted c
onnectivities');
#24943=UNCERTAINTY_MEASURE_WITH_UNIT(LENGTH_MEASURE(0.001),#25101,
'DISTANCE_ACCURACY_VALUE',
'Maximum model space distance between geometric entities at asserted c
onnectivities');
#24944=UNCERTAINTY_MEASURE_WITH_UNIT(LENGTH_MEASURE(0.001),#25101,
'DISTANCE_ACCURACY_VALUE',
'Maximum model space distance between geometric entities at asserted c
onnectivities');
#24945=UNCERTAINTY_MEASURE_WITH_UNIT(LENGTH_MEASURE(0.001),#25101,
'DISTANCE_ACCURACY_VALUE',
'Maximum model space distance between geometric entities at asserted c
onnectivities');
#24946=UNCERTAINTY_MEASURE_WITH_UNIT(LENGTH_MEASURE(0.001),#25101,
'DISTANCE_ACCURACY_VALUE',
'Maximum model space distance between geometric entities at asserted c
onnectivities');
#24947=UNCERTAINTY_MEASURE_WITH_UNIT(LENGTH_MEASURE(0.001),#25101,
'DISTANCE_ACCURACY_VALUE',
'Maximum model space distance between geometric entities at asserted c
onnectivities');
#24948=UNCERTAINTY_MEASURE_WITH_UNIT(LENGTH_MEASURE(0.001),#25101,
'DISTANCE_ACCURACY_VALUE',
'Maximum model space distance between geometric entities at asserted c
onnectivities');
#24949=UNCERTAINTY_MEASURE_WITH_UNIT(LENGTH_MEASURE(0.001),#25101,
'DISTANCE_ACCURACY_VALUE',
'Maximum model space distance between geometric entities at asserted c
onnectivities');
#24950=UNCERTAINTY_MEASURE_WITH_UNIT(LENGTH_MEASURE(0.001),#25101,
'DISTANCE_ACCURACY_VALUE',
'Maximum model space distance between geometric entities at asserted c
onnectivities');
#24951=UNCERTAINTY_MEASURE_WITH_UNIT(LENGTH_MEASURE(0.001),#25101,
'DISTANCE_ACCURACY_VALUE',
'Maximum model space distance between geometric entities at asserted c
onnectivities');
#24952=UNCERTAINTY_MEASURE_WITH_UNIT(LENGTH_MEASURE(0.001),#25101,
'DISTANCE_ACCURACY_VALUE',
'Maximum model space distance between geometric entities at asserted c
onnectivities');
#24953=UNCERTAINTY_MEASURE_WITH_UNIT(LENGTH_MEASURE(0.001),#25101,
'DISTANCE_ACCURACY_VALUE',
'Maximum model space distance between geometric entities at asserted c
onnectivities');
#24954=UNCERTAINTY_MEASURE_WITH_UNIT(LENGTH_MEASURE(0.001),#25101,
'DISTANCE_ACCURACY_VALUE',
'Maximum model space distance between geometric entities at asserted c
onnectivities');
#24955=UNCERTAINTY_MEASURE_WITH_UNIT(LENGTH_MEASURE(0.001),#25101,
'DISTANCE_ACCURACY_VALUE',
'Maximum model space distance between geometric entities at asserted c
onnectivities');
#24956=UNCERTAINTY_MEASURE_WITH_UNIT(LENGTH_MEASURE(0.001),#25101,
'DISTANCE_ACCURACY_VALUE',
'Maximum model space distance between geometric entities at asserted c
onnectivities');
#24957=UNCERTAINTY_MEASURE_WITH_UNIT(LENGTH_MEASURE(0.001),#25101,
'DISTANCE_ACCURACY_VALUE',
'Maximum model space distance between geometric entities at asserted c
onnectivities');
#24958=UNCERTAINTY_MEASURE_WITH_UNIT(LENGTH_MEASURE(0.001),#25101,
'DISTANCE_ACCURACY_VALUE',
'Maximum model space distance between geometric entities at asserted c
onnectivities');
#24959=UNCERTAINTY_MEASURE_WITH_UNIT(LENGTH_MEASURE(0.001),#25101,
'DISTANCE_ACCURACY_VALUE',
'Maximum model space distance between geometric entities at asserted c
onnectivities');
#24960=UNCERTAINTY_MEASURE_WITH_UNIT(LENGTH_MEASURE(0.001),#25101,
'DISTANCE_ACCURACY_VALUE',
'Maximum model space distance between geometric entities at asserted c
onnectivities');
#24961=UNCERTAINTY_MEASURE_WITH_UNIT(LENGTH_MEASURE(0.001),#25101,
'DISTANCE_ACCURACY_VALUE',
'Maximum model space distance between geometric entities at asserted c
onnectivities');
#24962=UNCERTAINTY_MEASURE_WITH_UNIT(LENGTH_MEASURE(0.001),#25101,
'DISTANCE_ACCURACY_VALUE',
'Maximum model space distance between geometric entities at asserted c
onnectivities');
#24963=UNCERTAINTY_MEASURE_WITH_UNIT(LENGTH_MEASURE(0.001),#25101,
'DISTANCE_ACCURACY_VALUE',
'Maximum model space distance between geometric entities at asserted c
onnectivities');
#24964=UNCERTAINTY_MEASURE_WITH_UNIT(LENGTH_MEASURE(0.001),#25101,
'DISTANCE_ACCURACY_VALUE',
'Maximum model space distance between geometric entities at asserted c
onnectivities');
#24965=UNCERTAINTY_MEASURE_WITH_UNIT(LENGTH_MEASURE(0.001),#25101,
'DISTANCE_ACCURACY_VALUE',
'Maximum model space distance between geometric entities at asserted c
onnectivities');
#24966=UNCERTAINTY_MEASURE_WITH_UNIT(LENGTH_MEASURE(0.001),#25101,
'DISTANCE_ACCURACY_VALUE',
'Maximum model space distance between geometric entities at asserted c
onnectivities');
#24967=UNCERTAINTY_MEASURE_WITH_UNIT(LENGTH_MEASURE(0.001),#25101,
'DISTANCE_ACCURACY_VALUE',
'Maximum model space distance between geometric entities at asserted c
onnectivities');
#24968=UNCERTAINTY_MEASURE_WITH_UNIT(LENGTH_MEASURE(0.001),#25101,
'DISTANCE_ACCURACY_VALUE',
'Maximum model space distance between geometric entities at asserted c
onnectivities');
#24969=UNCERTAINTY_MEASURE_WITH_UNIT(LENGTH_MEASURE(0.001),#25101,
'DISTANCE_ACCURACY_VALUE',
'Maximum model space distance between geometric entities at asserted c
onnectivities');
#24970=UNCERTAINTY_MEASURE_WITH_UNIT(LENGTH_MEASURE(0.001),#25101,
'DISTANCE_ACCURACY_VALUE',
'Maximum model space distance between geometric entities at asserted c
onnectivities');
#24971=UNCERTAINTY_MEASURE_WITH_UNIT(LENGTH_MEASURE(0.001),#25101,
'DISTANCE_ACCURACY_VALUE',
'Maximum model space distance between geometric entities at asserted c
onnectivities');
#24972=UNCERTAINTY_MEASURE_WITH_UNIT(LENGTH_MEASURE(0.001),#25101,
'DISTANCE_ACCURACY_VALUE',
'Maximum model space distance between geometric entities at asserted c
onnectivities');
#24973=UNCERTAINTY_MEASURE_WITH_UNIT(LENGTH_MEASURE(0.001),#25101,
'DISTANCE_ACCURACY_VALUE',
'Maximum model space distance between geometric entities at asserted c
onnectivities');
#24974=UNCERTAINTY_MEASURE_WITH_UNIT(LENGTH_MEASURE(0.001),#25101,
'DISTANCE_ACCURACY_VALUE',
'Maximum model space distance between geometric entities at asserted c
onnectivities');
#24975=UNCERTAINTY_MEASURE_WITH_UNIT(LENGTH_MEASURE(0.001),#25101,
'DISTANCE_ACCURACY_VALUE',
'Maximum model space distance between geometric entities at asserted c
onnectivities');
#24976=UNCERTAINTY_MEASURE_WITH_UNIT(LENGTH_MEASURE(0.001),#25101,
'DISTANCE_ACCURACY_VALUE',
'Maximum model space distance between geometric entities at asserted c
onnectivities');
#24977=UNCERTAINTY_MEASURE_WITH_UNIT(LENGTH_MEASURE(0.001),#25101,
'DISTANCE_ACCURACY_VALUE',
'Maximum model space distance between geometric entities at asserted c
onnectivities');
#24978=UNCERTAINTY_MEASURE_WITH_UNIT(LENGTH_MEASURE(0.001),#25101,
'DISTANCE_ACCURACY_VALUE',
'Maximum model space distance between geometric entities at asserted c
onnectivities');
#24979=UNCERTAINTY_MEASURE_WITH_UNIT(LENGTH_MEASURE(0.001),#25101,
'DISTANCE_ACCURACY_VALUE',
'Maximum model space distance between geometric entities at asserted c
onnectivities');
#24980=(
GEOMETRIC_REPRESENTATION_CONTEXT(3)
GLOBAL_UNCERTAINTY_ASSIGNED_CONTEXT((#24859))
GLOBAL_UNIT_ASSIGNED_CONTEXT((#25101,#25103,#25104))
REPRESENTATION_CONTEXT('','3D')
);
#24981=(
GEOMETRIC_REPRESENTATION_CONTEXT(3)
GLOBAL_UNCERTAINTY_ASSIGNED_CONTEXT((#24860))
GLOBAL_UNIT_ASSIGNED_CONTEXT((#25101,#25103,#25104))
REPRESENTATION_CONTEXT('','3D')
);
#24982=(
GEOMETRIC_REPRESENTATION_CONTEXT(3)
GLOBAL_UNCERTAINTY_ASSIGNED_CONTEXT((#24861))
GLOBAL_UNIT_ASSIGNED_CONTEXT((#25101,#25103,#25104))
REPRESENTATION_CONTEXT('','3D')
);
#24983=(
GEOMETRIC_REPRESENTATION_CONTEXT(3)
GLOBAL_UNCERTAINTY_ASSIGNED_CONTEXT((#24862))
GLOBAL_UNIT_ASSIGNED_CONTEXT((#25101,#25103,#25104))
REPRESENTATION_CONTEXT('','3D')
);
#24984=(
GEOMETRIC_REPRESENTATION_CONTEXT(3)
GLOBAL_UNCERTAINTY_ASSIGNED_CONTEXT((#24863))
GLOBAL_UNIT_ASSIGNED_CONTEXT((#25101,#25103,#25104))
REPRESENTATION_CONTEXT('','3D')
);
#24985=(
GEOMETRIC_REPRESENTATION_CONTEXT(3)
GLOBAL_UNCERTAINTY_ASSIGNED_CONTEXT((#24864))
GLOBAL_UNIT_ASSIGNED_CONTEXT((#25101,#25103,#25104))
REPRESENTATION_CONTEXT('','3D')
);
#24986=(
GEOMETRIC_REPRESENTATION_CONTEXT(3)
GLOBAL_UNCERTAINTY_ASSIGNED_CONTEXT((#24865))
GLOBAL_UNIT_ASSIGNED_CONTEXT((#25101,#25103,#25104))
REPRESENTATION_CONTEXT('','3D')
);
#24987=(
GEOMETRIC_REPRESENTATION_CONTEXT(3)
GLOBAL_UNCERTAINTY_ASSIGNED_CONTEXT((#24866))
GLOBAL_UNIT_ASSIGNED_CONTEXT((#25101,#25103,#25104))
REPRESENTATION_CONTEXT('','3D')
);
#24988=(
GEOMETRIC_REPRESENTATION_CONTEXT(3)
GLOBAL_UNCERTAINTY_ASSIGNED_CONTEXT((#24867))
GLOBAL_UNIT_ASSIGNED_CONTEXT((#25101,#25103,#25104))
REPRESENTATION_CONTEXT('','3D')
);
#24989=(
GEOMETRIC_REPRESENTATION_CONTEXT(3)
GLOBAL_UNCERTAINTY_ASSIGNED_CONTEXT((#24868))
GLOBAL_UNIT_ASSIGNED_CONTEXT((#25101,#25103,#25104))
REPRESENTATION_CONTEXT('','3D')
);
#24990=(
GEOMETRIC_REPRESENTATION_CONTEXT(3)
GLOBAL_UNCERTAINTY_ASSIGNED_CONTEXT((#24869))
GLOBAL_UNIT_ASSIGNED_CONTEXT((#25101,#25103,#25104))
REPRESENTATION_CONTEXT('','3D')
);
#24991=(
GEOMETRIC_REPRESENTATION_CONTEXT(3)
GLOBAL_UNCERTAINTY_ASSIGNED_CONTEXT((#24870))
GLOBAL_UNIT_ASSIGNED_CONTEXT((#25101,#25103,#25104))
REPRESENTATION_CONTEXT('','3D')
);
#24992=(
GEOMETRIC_REPRESENTATION_CONTEXT(3)
GLOBAL_UNCERTAINTY_ASSIGNED_CONTEXT((#24871))
GLOBAL_UNIT_ASSIGNED_CONTEXT((#25101,#25103,#25104))
REPRESENTATION_CONTEXT('','3D')
);
#24993=(
GEOMETRIC_REPRESENTATION_CONTEXT(3)
GLOBAL_UNCERTAINTY_ASSIGNED_CONTEXT((#24872))
GLOBAL_UNIT_ASSIGNED_CONTEXT((#25101,#25103,#25104))
REPRESENTATION_CONTEXT('','3D')
);
#24994=(
GEOMETRIC_REPRESENTATION_CONTEXT(3)
GLOBAL_UNCERTAINTY_ASSIGNED_CONTEXT((#24873))
GLOBAL_UNIT_ASSIGNED_CONTEXT((#25101,#25103,#25104))
REPRESENTATION_CONTEXT('','3D')
);
#24995=(
GEOMETRIC_REPRESENTATION_CONTEXT(3)
GLOBAL_UNCERTAINTY_ASSIGNED_CONTEXT((#24874))
GLOBAL_UNIT_ASSIGNED_CONTEXT((#25101,#25103,#25104))
REPRESENTATION_CONTEXT('','3D')
);
#24996=(
GEOMETRIC_REPRESENTATION_CONTEXT(3)
GLOBAL_UNCERTAINTY_ASSIGNED_CONTEXT((#24875))
GLOBAL_UNIT_ASSIGNED_CONTEXT((#25101,#25103,#25104))
REPRESENTATION_CONTEXT('','3D')
);
#24997=(
GEOMETRIC_REPRESENTATION_CONTEXT(3)
GLOBAL_UNCERTAINTY_ASSIGNED_CONTEXT((#24876))
GLOBAL_UNIT_ASSIGNED_CONTEXT((#25101,#25103,#25104))
REPRESENTATION_CONTEXT('','3D')
);
#24998=(
GEOMETRIC_REPRESENTATION_CONTEXT(3)
GLOBAL_UNCERTAINTY_ASSIGNED_CONTEXT((#24877))
GLOBAL_UNIT_ASSIGNED_CONTEXT((#25101,#25103,#25104))
REPRESENTATION_CONTEXT('','3D')
);
#24999=(
GEOMETRIC_REPRESENTATION_CONTEXT(3)
GLOBAL_UNCERTAINTY_ASSIGNED_CONTEXT((#24878))
GLOBAL_UNIT_ASSIGNED_CONTEXT((#25101,#25103,#25104))
REPRESENTATION_CONTEXT('','3D')
);
#25000=(
GEOMETRIC_REPRESENTATION_CONTEXT(3)
GLOBAL_UNCERTAINTY_ASSIGNED_CONTEXT((#24879))
GLOBAL_UNIT_ASSIGNED_CONTEXT((#25101,#25103,#25104))
REPRESENTATION_CONTEXT('','3D')
);
#25001=(
GEOMETRIC_REPRESENTATION_CONTEXT(3)
GLOBAL_UNCERTAINTY_ASSIGNED_CONTEXT((#24880))
GLOBAL_UNIT_ASSIGNED_CONTEXT((#25101,#25103,#25104))
REPRESENTATION_CONTEXT('','3D')
);
#25002=(
GEOMETRIC_REPRESENTATION_CONTEXT(3)
GLOBAL_UNCERTAINTY_ASSIGNED_CONTEXT((#24881))
GLOBAL_UNIT_ASSIGNED_CONTEXT((#25101,#25103,#25104))
REPRESENTATION_CONTEXT('','3D')
);
#25003=(
GEOMETRIC_REPRESENTATION_CONTEXT(3)
GLOBAL_UNCERTAINTY_ASSIGNED_CONTEXT((#24882))
GLOBAL_UNIT_ASSIGNED_CONTEXT((#25101,#25103,#25104))
REPRESENTATION_CONTEXT('','3D')
);
#25004=(
GEOMETRIC_REPRESENTATION_CONTEXT(3)
GLOBAL_UNCERTAINTY_ASSIGNED_CONTEXT((#24883))
GLOBAL_UNIT_ASSIGNED_CONTEXT((#25101,#25103,#25104))
REPRESENTATION_CONTEXT('','3D')
);
#25005=(
GEOMETRIC_REPRESENTATION_CONTEXT(3)
GLOBAL_UNCERTAINTY_ASSIGNED_CONTEXT((#24884))
GLOBAL_UNIT_ASSIGNED_CONTEXT((#25101,#25103,#25104))
REPRESENTATION_CONTEXT('','3D')
);
#25006=(
GEOMETRIC_REPRESENTATION_CONTEXT(3)
GLOBAL_UNCERTAINTY_ASSIGNED_CONTEXT((#24885))
GLOBAL_UNIT_ASSIGNED_CONTEXT((#25101,#25103,#25104))
REPRESENTATION_CONTEXT('','3D')
);
#25007=(
GEOMETRIC_REPRESENTATION_CONTEXT(3)
GLOBAL_UNCERTAINTY_ASSIGNED_CONTEXT((#24886))
GLOBAL_UNIT_ASSIGNED_CONTEXT((#25101,#25103,#25104))
REPRESENTATION_CONTEXT('','3D')
);
#25008=(
GEOMETRIC_REPRESENTATION_CONTEXT(3)
GLOBAL_UNCERTAINTY_ASSIGNED_CONTEXT((#24887))
GLOBAL_UNIT_ASSIGNED_CONTEXT((#25101,#25103,#25104))
REPRESENTATION_CONTEXT('','3D')
);
#25009=(
GEOMETRIC_REPRESENTATION_CONTEXT(3)
GLOBAL_UNCERTAINTY_ASSIGNED_CONTEXT((#24888))
GLOBAL_UNIT_ASSIGNED_CONTEXT((#25101,#25103,#25104))
REPRESENTATION_CONTEXT('','3D')
);
#25010=(
GEOMETRIC_REPRESENTATION_CONTEXT(3)
GLOBAL_UNCERTAINTY_ASSIGNED_CONTEXT((#24889))
GLOBAL_UNIT_ASSIGNED_CONTEXT((#25101,#25103,#25104))
REPRESENTATION_CONTEXT('','3D')
);
#25011=(
GEOMETRIC_REPRESENTATION_CONTEXT(3)
GLOBAL_UNCERTAINTY_ASSIGNED_CONTEXT((#24890))
GLOBAL_UNIT_ASSIGNED_CONTEXT((#25101,#25103,#25104))
REPRESENTATION_CONTEXT('','3D')
);
#25012=(
GEOMETRIC_REPRESENTATION_CONTEXT(3)
GLOBAL_UNCERTAINTY_ASSIGNED_CONTEXT((#24891))
GLOBAL_UNIT_ASSIGNED_CONTEXT((#25101,#25103,#25104))
REPRESENTATION_CONTEXT('','3D')
);
#25013=(
GEOMETRIC_REPRESENTATION_CONTEXT(3)
GLOBAL_UNCERTAINTY_ASSIGNED_CONTEXT((#24892))
GLOBAL_UNIT_ASSIGNED_CONTEXT((#25101,#25103,#25104))
REPRESENTATION_CONTEXT('','3D')
);
#25014=(
GEOMETRIC_REPRESENTATION_CONTEXT(3)
GLOBAL_UNCERTAINTY_ASSIGNED_CONTEXT((#24893))
GLOBAL_UNIT_ASSIGNED_CONTEXT((#25101,#25103,#25104))
REPRESENTATION_CONTEXT('','3D')
);
#25015=(
GEOMETRIC_REPRESENTATION_CONTEXT(3)
GLOBAL_UNCERTAINTY_ASSIGNED_CONTEXT((#24894))
GLOBAL_UNIT_ASSIGNED_CONTEXT((#25101,#25103,#25104))
REPRESENTATION_CONTEXT('','3D')
);
#25016=(
GEOMETRIC_REPRESENTATION_CONTEXT(3)
GLOBAL_UNCERTAINTY_ASSIGNED_CONTEXT((#24895))
GLOBAL_UNIT_ASSIGNED_CONTEXT((#25101,#25103,#25104))
REPRESENTATION_CONTEXT('','3D')
);
#25017=(
GEOMETRIC_REPRESENTATION_CONTEXT(3)
GLOBAL_UNCERTAINTY_ASSIGNED_CONTEXT((#24896))
GLOBAL_UNIT_ASSIGNED_CONTEXT((#25101,#25103,#25104))
REPRESENTATION_CONTEXT('','3D')
);
#25018=(
GEOMETRIC_REPRESENTATION_CONTEXT(3)
GLOBAL_UNCERTAINTY_ASSIGNED_CONTEXT((#24897))
GLOBAL_UNIT_ASSIGNED_CONTEXT((#25101,#25103,#25104))
REPRESENTATION_CONTEXT('','3D')
);
#25019=(
GEOMETRIC_REPRESENTATION_CONTEXT(3)
GLOBAL_UNCERTAINTY_ASSIGNED_CONTEXT((#24898))
GLOBAL_UNIT_ASSIGNED_CONTEXT((#25101,#25103,#25104))
REPRESENTATION_CONTEXT('','3D')
);
#25020=(
GEOMETRIC_REPRESENTATION_CONTEXT(3)
GLOBAL_UNCERTAINTY_ASSIGNED_CONTEXT((#24899))
GLOBAL_UNIT_ASSIGNED_CONTEXT((#25101,#25103,#25104))
REPRESENTATION_CONTEXT('','3D')
);
#25021=(
GEOMETRIC_REPRESENTATION_CONTEXT(3)
GLOBAL_UNCERTAINTY_ASSIGNED_CONTEXT((#24900))
GLOBAL_UNIT_ASSIGNED_CONTEXT((#25101,#25103,#25104))
REPRESENTATION_CONTEXT('','3D')
);
#25022=(
GEOMETRIC_REPRESENTATION_CONTEXT(3)
GLOBAL_UNCERTAINTY_ASSIGNED_CONTEXT((#24901))
GLOBAL_UNIT_ASSIGNED_CONTEXT((#25101,#25103,#25104))
REPRESENTATION_CONTEXT('','3D')
);
#25023=(
GEOMETRIC_REPRESENTATION_CONTEXT(3)
GLOBAL_UNCERTAINTY_ASSIGNED_CONTEXT((#24902))
GLOBAL_UNIT_ASSIGNED_CONTEXT((#25101,#25103,#25104))
REPRESENTATION_CONTEXT('','3D')
);
#25024=(
GEOMETRIC_REPRESENTATION_CONTEXT(3)
GLOBAL_UNCERTAINTY_ASSIGNED_CONTEXT((#24903))
GLOBAL_UNIT_ASSIGNED_CONTEXT((#25101,#25103,#25104))
REPRESENTATION_CONTEXT('','3D')
);
#25025=(
GEOMETRIC_REPRESENTATION_CONTEXT(3)
GLOBAL_UNCERTAINTY_ASSIGNED_CONTEXT((#24904))
GLOBAL_UNIT_ASSIGNED_CONTEXT((#25101,#25103,#25104))
REPRESENTATION_CONTEXT('','3D')
);
#25026=(
GEOMETRIC_REPRESENTATION_CONTEXT(3)
GLOBAL_UNCERTAINTY_ASSIGNED_CONTEXT((#24905))
GLOBAL_UNIT_ASSIGNED_CONTEXT((#25101,#25103,#25104))
REPRESENTATION_CONTEXT('','3D')
);
#25027=(
GEOMETRIC_REPRESENTATION_CONTEXT(3)
GLOBAL_UNCERTAINTY_ASSIGNED_CONTEXT((#24906))
GLOBAL_UNIT_ASSIGNED_CONTEXT((#25101,#25103,#25104))
REPRESENTATION_CONTEXT('','3D')
);
#25028=(
GEOMETRIC_REPRESENTATION_CONTEXT(3)
GLOBAL_UNCERTAINTY_ASSIGNED_CONTEXT((#24907))
GLOBAL_UNIT_ASSIGNED_CONTEXT((#25101,#25103,#25104))
REPRESENTATION_CONTEXT('','3D')
);
#25029=(
GEOMETRIC_REPRESENTATION_CONTEXT(3)
GLOBAL_UNCERTAINTY_ASSIGNED_CONTEXT((#24908))
GLOBAL_UNIT_ASSIGNED_CONTEXT((#25101,#25103,#25104))
REPRESENTATION_CONTEXT('','3D')
);
#25030=(
GEOMETRIC_REPRESENTATION_CONTEXT(3)
GLOBAL_UNCERTAINTY_ASSIGNED_CONTEXT((#24909))
GLOBAL_UNIT_ASSIGNED_CONTEXT((#25101,#25103,#25104))
REPRESENTATION_CONTEXT('','3D')
);
#25031=(
GEOMETRIC_REPRESENTATION_CONTEXT(3)
GLOBAL_UNCERTAINTY_ASSIGNED_CONTEXT((#24910))
GLOBAL_UNIT_ASSIGNED_CONTEXT((#25101,#25103,#25104))
REPRESENTATION_CONTEXT('','3D')
);
#25032=(
GEOMETRIC_REPRESENTATION_CONTEXT(3)
GLOBAL_UNCERTAINTY_ASSIGNED_CONTEXT((#24911))
GLOBAL_UNIT_ASSIGNED_CONTEXT((#25101,#25103,#25104))
REPRESENTATION_CONTEXT('','3D')
);
#25033=(
GEOMETRIC_REPRESENTATION_CONTEXT(3)
GLOBAL_UNCERTAINTY_ASSIGNED_CONTEXT((#24912))
GLOBAL_UNIT_ASSIGNED_CONTEXT((#25101,#25103,#25104))
REPRESENTATION_CONTEXT('','3D')
);
#25034=(
GEOMETRIC_REPRESENTATION_CONTEXT(3)
GLOBAL_UNCERTAINTY_ASSIGNED_CONTEXT((#24913))
GLOBAL_UNIT_ASSIGNED_CONTEXT((#25101,#25103,#25104))
REPRESENTATION_CONTEXT('','3D')
);
#25035=(
GEOMETRIC_REPRESENTATION_CONTEXT(3)
GLOBAL_UNCERTAINTY_ASSIGNED_CONTEXT((#24914))
GLOBAL_UNIT_ASSIGNED_CONTEXT((#25101,#25103,#25104))
REPRESENTATION_CONTEXT('','3D')
);
#25036=(
GEOMETRIC_REPRESENTATION_CONTEXT(3)
GLOBAL_UNCERTAINTY_ASSIGNED_CONTEXT((#24915))
GLOBAL_UNIT_ASSIGNED_CONTEXT((#25101,#25103,#25104))
REPRESENTATION_CONTEXT('','3D')
);
#25037=(
GEOMETRIC_REPRESENTATION_CONTEXT(3)
GLOBAL_UNCERTAINTY_ASSIGNED_CONTEXT((#24916))
GLOBAL_UNIT_ASSIGNED_CONTEXT((#25101,#25103,#25104))
REPRESENTATION_CONTEXT('','3D')
);
#25038=(
GEOMETRIC_REPRESENTATION_CONTEXT(3)
GLOBAL_UNCERTAINTY_ASSIGNED_CONTEXT((#24917))
GLOBAL_UNIT_ASSIGNED_CONTEXT((#25101,#25103,#25104))
REPRESENTATION_CONTEXT('','3D')
);
#25039=(
GEOMETRIC_REPRESENTATION_CONTEXT(3)
GLOBAL_UNCERTAINTY_ASSIGNED_CONTEXT((#24918))
GLOBAL_UNIT_ASSIGNED_CONTEXT((#25101,#25103,#25104))
REPRESENTATION_CONTEXT('','3D')
);
#25040=(
GEOMETRIC_REPRESENTATION_CONTEXT(3)
GLOBAL_UNCERTAINTY_ASSIGNED_CONTEXT((#24919))
GLOBAL_UNIT_ASSIGNED_CONTEXT((#25101,#25103,#25104))
REPRESENTATION_CONTEXT('','3D')
);
#25041=(
GEOMETRIC_REPRESENTATION_CONTEXT(3)
GLOBAL_UNCERTAINTY_ASSIGNED_CONTEXT((#24920))
GLOBAL_UNIT_ASSIGNED_CONTEXT((#25101,#25103,#25104))
REPRESENTATION_CONTEXT('','3D')
);
#25042=(
GEOMETRIC_REPRESENTATION_CONTEXT(3)
GLOBAL_UNCERTAINTY_ASSIGNED_CONTEXT((#24921))
GLOBAL_UNIT_ASSIGNED_CONTEXT((#25101,#25103,#25104))
REPRESENTATION_CONTEXT('','3D')
);
#25043=(
GEOMETRIC_REPRESENTATION_CONTEXT(3)
GLOBAL_UNCERTAINTY_ASSIGNED_CONTEXT((#24922))
GLOBAL_UNIT_ASSIGNED_CONTEXT((#25101,#25103,#25104))
REPRESENTATION_CONTEXT('','3D')
);
#25044=(
GEOMETRIC_REPRESENTATION_CONTEXT(3)
GLOBAL_UNCERTAINTY_ASSIGNED_CONTEXT((#24923))
GLOBAL_UNIT_ASSIGNED_CONTEXT((#25101,#25103,#25104))
REPRESENTATION_CONTEXT('','3D')
);
#25045=(
GEOMETRIC_REPRESENTATION_CONTEXT(3)
GLOBAL_UNCERTAINTY_ASSIGNED_CONTEXT((#24924))
GLOBAL_UNIT_ASSIGNED_CONTEXT((#25101,#25103,#25104))
REPRESENTATION_CONTEXT('','3D')
);
#25046=(
GEOMETRIC_REPRESENTATION_CONTEXT(3)
GLOBAL_UNCERTAINTY_ASSIGNED_CONTEXT((#24925))
GLOBAL_UNIT_ASSIGNED_CONTEXT((#25101,#25103,#25104))
REPRESENTATION_CONTEXT('','3D')
);
#25047=(
GEOMETRIC_REPRESENTATION_CONTEXT(3)
GLOBAL_UNCERTAINTY_ASSIGNED_CONTEXT((#24926))
GLOBAL_UNIT_ASSIGNED_CONTEXT((#25101,#25103,#25104))
REPRESENTATION_CONTEXT('','3D')
);
#25048=(
GEOMETRIC_REPRESENTATION_CONTEXT(3)
GLOBAL_UNCERTAINTY_ASSIGNED_CONTEXT((#24927))
GLOBAL_UNIT_ASSIGNED_CONTEXT((#25101,#25103,#25104))
REPRESENTATION_CONTEXT('','3D')
);
#25049=(
GEOMETRIC_REPRESENTATION_CONTEXT(3)
GLOBAL_UNCERTAINTY_ASSIGNED_CONTEXT((#24928))
GLOBAL_UNIT_ASSIGNED_CONTEXT((#25101,#25103,#25104))
REPRESENTATION_CONTEXT('','3D')
);
#25050=(
GEOMETRIC_REPRESENTATION_CONTEXT(3)
GLOBAL_UNCERTAINTY_ASSIGNED_CONTEXT((#24929))
GLOBAL_UNIT_ASSIGNED_CONTEXT((#25101,#25103,#25104))
REPRESENTATION_CONTEXT('','3D')
);
#25051=(
GEOMETRIC_REPRESENTATION_CONTEXT(3)
GLOBAL_UNCERTAINTY_ASSIGNED_CONTEXT((#24930))
GLOBAL_UNIT_ASSIGNED_CONTEXT((#25101,#25103,#25104))
REPRESENTATION_CONTEXT('','3D')
);
#25052=(
GEOMETRIC_REPRESENTATION_CONTEXT(3)
GLOBAL_UNCERTAINTY_ASSIGNED_CONTEXT((#24931))
GLOBAL_UNIT_ASSIGNED_CONTEXT((#25101,#25103,#25104))
REPRESENTATION_CONTEXT('','3D')
);
#25053=(
GEOMETRIC_REPRESENTATION_CONTEXT(3)
GLOBAL_UNCERTAINTY_ASSIGNED_CONTEXT((#24932))
GLOBAL_UNIT_ASSIGNED_CONTEXT((#25101,#25103,#25104))
REPRESENTATION_CONTEXT('','3D')
);
#25054=(
GEOMETRIC_REPRESENTATION_CONTEXT(3)
GLOBAL_UNCERTAINTY_ASSIGNED_CONTEXT((#24933))
GLOBAL_UNIT_ASSIGNED_CONTEXT((#25101,#25103,#25104))
REPRESENTATION_CONTEXT('','3D')
);
#25055=(
GEOMETRIC_REPRESENTATION_CONTEXT(3)
GLOBAL_UNCERTAINTY_ASSIGNED_CONTEXT((#24934))
GLOBAL_UNIT_ASSIGNED_CONTEXT((#25101,#25103,#25104))
REPRESENTATION_CONTEXT('','3D')
);
#25056=(
GEOMETRIC_REPRESENTATION_CONTEXT(3)
GLOBAL_UNCERTAINTY_ASSIGNED_CONTEXT((#24935))
GLOBAL_UNIT_ASSIGNED_CONTEXT((#25101,#25103,#25104))
REPRESENTATION_CONTEXT('','3D')
);
#25057=(
GEOMETRIC_REPRESENTATION_CONTEXT(3)
GLOBAL_UNCERTAINTY_ASSIGNED_CONTEXT((#24936))
GLOBAL_UNIT_ASSIGNED_CONTEXT((#25101,#25103,#25104))
REPRESENTATION_CONTEXT('','3D')
);
#25058=(
GEOMETRIC_REPRESENTATION_CONTEXT(3)
GLOBAL_UNCERTAINTY_ASSIGNED_CONTEXT((#24937))
GLOBAL_UNIT_ASSIGNED_CONTEXT((#25101,#25103,#25104))
REPRESENTATION_CONTEXT('','3D')
);
#25059=(
GEOMETRIC_REPRESENTATION_CONTEXT(3)
GLOBAL_UNCERTAINTY_ASSIGNED_CONTEXT((#24938))
GLOBAL_UNIT_ASSIGNED_CONTEXT((#25101,#25103,#25104))
REPRESENTATION_CONTEXT('','3D')
);
#25060=(
GEOMETRIC_REPRESENTATION_CONTEXT(3)
GLOBAL_UNCERTAINTY_ASSIGNED_CONTEXT((#24939))
GLOBAL_UNIT_ASSIGNED_CONTEXT((#25101,#25103,#25104))
REPRESENTATION_CONTEXT('','3D')
);
#25061=(
GEOMETRIC_REPRESENTATION_CONTEXT(3)
GLOBAL_UNCERTAINTY_ASSIGNED_CONTEXT((#24940))
GLOBAL_UNIT_ASSIGNED_CONTEXT((#25101,#25103,#25104))
REPRESENTATION_CONTEXT('','3D')
);
#25062=(
GEOMETRIC_REPRESENTATION_CONTEXT(3)
GLOBAL_UNCERTAINTY_ASSIGNED_CONTEXT((#24941))
GLOBAL_UNIT_ASSIGNED_CONTEXT((#25101,#25103,#25104))
REPRESENTATION_CONTEXT('','3D')
);
#25063=(
GEOMETRIC_REPRESENTATION_CONTEXT(3)
GLOBAL_UNCERTAINTY_ASSIGNED_CONTEXT((#24942))
GLOBAL_UNIT_ASSIGNED_CONTEXT((#25101,#25103,#25104))
REPRESENTATION_CONTEXT('','3D')
);
#25064=(
GEOMETRIC_REPRESENTATION_CONTEXT(3)
GLOBAL_UNCERTAINTY_ASSIGNED_CONTEXT((#24943))
GLOBAL_UNIT_ASSIGNED_CONTEXT((#25101,#25103,#25104))
REPRESENTATION_CONTEXT('','3D')
);
#25065=(
GEOMETRIC_REPRESENTATION_CONTEXT(3)
GLOBAL_UNCERTAINTY_ASSIGNED_CONTEXT((#24944))
GLOBAL_UNIT_ASSIGNED_CONTEXT((#25101,#25103,#25104))
REPRESENTATION_CONTEXT('','3D')
);
#25066=(
GEOMETRIC_REPRESENTATION_CONTEXT(3)
GLOBAL_UNCERTAINTY_ASSIGNED_CONTEXT((#24945))
GLOBAL_UNIT_ASSIGNED_CONTEXT((#25101,#25103,#25104))
REPRESENTATION_CONTEXT('','3D')
);
#25067=(
GEOMETRIC_REPRESENTATION_CONTEXT(3)
GLOBAL_UNCERTAINTY_ASSIGNED_CONTEXT((#24946))
GLOBAL_UNIT_ASSIGNED_CONTEXT((#25101,#25103,#25104))
REPRESENTATION_CONTEXT('','3D')
);
#25068=(
GEOMETRIC_REPRESENTATION_CONTEXT(3)
GLOBAL_UNCERTAINTY_ASSIGNED_CONTEXT((#24947))
GLOBAL_UNIT_ASSIGNED_CONTEXT((#25101,#25103,#25104))
REPRESENTATION_CONTEXT('','3D')
);
#25069=(
GEOMETRIC_REPRESENTATION_CONTEXT(3)
GLOBAL_UNCERTAINTY_ASSIGNED_CONTEXT((#24948))
GLOBAL_UNIT_ASSIGNED_CONTEXT((#25101,#25103,#25104))
REPRESENTATION_CONTEXT('','3D')
);
#25070=(
GEOMETRIC_REPRESENTATION_CONTEXT(3)
GLOBAL_UNCERTAINTY_ASSIGNED_CONTEXT((#24949))
GLOBAL_UNIT_ASSIGNED_CONTEXT((#25101,#25103,#25104))
REPRESENTATION_CONTEXT('','3D')
);
#25071=(
GEOMETRIC_REPRESENTATION_CONTEXT(3)
GLOBAL_UNCERTAINTY_ASSIGNED_CONTEXT((#24950))
GLOBAL_UNIT_ASSIGNED_CONTEXT((#25101,#25103,#25104))
REPRESENTATION_CONTEXT('','3D')
);
#25072=(
GEOMETRIC_REPRESENTATION_CONTEXT(3)
GLOBAL_UNCERTAINTY_ASSIGNED_CONTEXT((#24951))
GLOBAL_UNIT_ASSIGNED_CONTEXT((#25101,#25103,#25104))
REPRESENTATION_CONTEXT('','3D')
);
#25073=(
GEOMETRIC_REPRESENTATION_CONTEXT(3)
GLOBAL_UNCERTAINTY_ASSIGNED_CONTEXT((#24952))
GLOBAL_UNIT_ASSIGNED_CONTEXT((#25101,#25103,#25104))
REPRESENTATION_CONTEXT('','3D')
);
#25074=(
GEOMETRIC_REPRESENTATION_CONTEXT(3)
GLOBAL_UNCERTAINTY_ASSIGNED_CONTEXT((#24953))
GLOBAL_UNIT_ASSIGNED_CONTEXT((#25101,#25103,#25104))
REPRESENTATION_CONTEXT('','3D')
);
#25075=(
GEOMETRIC_REPRESENTATION_CONTEXT(3)
GLOBAL_UNCERTAINTY_ASSIGNED_CONTEXT((#24954))
GLOBAL_UNIT_ASSIGNED_CONTEXT((#25101,#25103,#25104))
REPRESENTATION_CONTEXT('','3D')
);
#25076=(
GEOMETRIC_REPRESENTATION_CONTEXT(3)
GLOBAL_UNCERTAINTY_ASSIGNED_CONTEXT((#24955))
GLOBAL_UNIT_ASSIGNED_CONTEXT((#25101,#25103,#25104))
REPRESENTATION_CONTEXT('','3D')
);
#25077=(
GEOMETRIC_REPRESENTATION_CONTEXT(3)
GLOBAL_UNCERTAINTY_ASSIGNED_CONTEXT((#24956))
GLOBAL_UNIT_ASSIGNED_CONTEXT((#25101,#25103,#25104))
REPRESENTATION_CONTEXT('','3D')
);
#25078=(
GEOMETRIC_REPRESENTATION_CONTEXT(3)
GLOBAL_UNCERTAINTY_ASSIGNED_CONTEXT((#24957))
GLOBAL_UNIT_ASSIGNED_CONTEXT((#25101,#25103,#25104))
REPRESENTATION_CONTEXT('','3D')
);
#25079=(
GEOMETRIC_REPRESENTATION_CONTEXT(3)
GLOBAL_UNCERTAINTY_ASSIGNED_CONTEXT((#24958))
GLOBAL_UNIT_ASSIGNED_CONTEXT((#25101,#25103,#25104))
REPRESENTATION_CONTEXT('','3D')
);
#25080=(
GEOMETRIC_REPRESENTATION_CONTEXT(3)
GLOBAL_UNCERTAINTY_ASSIGNED_CONTEXT((#24959))
GLOBAL_UNIT_ASSIGNED_CONTEXT((#25101,#25103,#25104))
REPRESENTATION_CONTEXT('','3D')
);
#25081=(
GEOMETRIC_REPRESENTATION_CONTEXT(3)
GLOBAL_UNCERTAINTY_ASSIGNED_CONTEXT((#24960))
GLOBAL_UNIT_ASSIGNED_CONTEXT((#25101,#25103,#25104))
REPRESENTATION_CONTEXT('','3D')
);
#25082=(
GEOMETRIC_REPRESENTATION_CONTEXT(3)
GLOBAL_UNCERTAINTY_ASSIGNED_CONTEXT((#24961))
GLOBAL_UNIT_ASSIGNED_CONTEXT((#25101,#25103,#25104))
REPRESENTATION_CONTEXT('','3D')
);
#25083=(
GEOMETRIC_REPRESENTATION_CONTEXT(3)
GLOBAL_UNCERTAINTY_ASSIGNED_CONTEXT((#24962))
GLOBAL_UNIT_ASSIGNED_CONTEXT((#25101,#25103,#25104))
REPRESENTATION_CONTEXT('','3D')
);
#25084=(
GEOMETRIC_REPRESENTATION_CONTEXT(3)
GLOBAL_UNCERTAINTY_ASSIGNED_CONTEXT((#24963))
GLOBAL_UNIT_ASSIGNED_CONTEXT((#25101,#25103,#25104))
REPRESENTATION_CONTEXT('','3D')
);
#25085=(
GEOMETRIC_REPRESENTATION_CONTEXT(3)
GLOBAL_UNCERTAINTY_ASSIGNED_CONTEXT((#24964))
GLOBAL_UNIT_ASSIGNED_CONTEXT((#25101,#25103,#25104))
REPRESENTATION_CONTEXT('','3D')
);
#25086=(
GEOMETRIC_REPRESENTATION_CONTEXT(3)
GLOBAL_UNCERTAINTY_ASSIGNED_CONTEXT((#24965))
GLOBAL_UNIT_ASSIGNED_CONTEXT((#25101,#25103,#25104))
REPRESENTATION_CONTEXT('','3D')
);
#25087=(
GEOMETRIC_REPRESENTATION_CONTEXT(3)
GLOBAL_UNCERTAINTY_ASSIGNED_CONTEXT((#24966))
GLOBAL_UNIT_ASSIGNED_CONTEXT((#25101,#25103,#25104))
REPRESENTATION_CONTEXT('','3D')
);
#25088=(
GEOMETRIC_REPRESENTATION_CONTEXT(3)
GLOBAL_UNCERTAINTY_ASSIGNED_CONTEXT((#24967))
GLOBAL_UNIT_ASSIGNED_CONTEXT((#25101,#25103,#25104))
REPRESENTATION_CONTEXT('','3D')
);
#25089=(
GEOMETRIC_REPRESENTATION_CONTEXT(3)
GLOBAL_UNCERTAINTY_ASSIGNED_CONTEXT((#24968))
GLOBAL_UNIT_ASSIGNED_CONTEXT((#25101,#25103,#25104))
REPRESENTATION_CONTEXT('','3D')
);
#25090=(
GEOMETRIC_REPRESENTATION_CONTEXT(3)
GLOBAL_UNCERTAINTY_ASSIGNED_CONTEXT((#24969))
GLOBAL_UNIT_ASSIGNED_CONTEXT((#25101,#25103,#25104))
REPRESENTATION_CONTEXT('','3D')
);
#25091=(
GEOMETRIC_REPRESENTATION_CONTEXT(3)
GLOBAL_UNCERTAINTY_ASSIGNED_CONTEXT((#24970))
GLOBAL_UNIT_ASSIGNED_CONTEXT((#25101,#25103,#25104))
REPRESENTATION_CONTEXT('','3D')
);
#25092=(
GEOMETRIC_REPRESENTATION_CONTEXT(3)
GLOBAL_UNCERTAINTY_ASSIGNED_CONTEXT((#24971))
GLOBAL_UNIT_ASSIGNED_CONTEXT((#25101,#25103,#25104))
REPRESENTATION_CONTEXT('','3D')
);
#25093=(
GEOMETRIC_REPRESENTATION_CONTEXT(3)
GLOBAL_UNCERTAINTY_ASSIGNED_CONTEXT((#24972))
GLOBAL_UNIT_ASSIGNED_CONTEXT((#25101,#25103,#25104))
REPRESENTATION_CONTEXT('','3D')
);
#25094=(
GEOMETRIC_REPRESENTATION_CONTEXT(3)
GLOBAL_UNCERTAINTY_ASSIGNED_CONTEXT((#24973))
GLOBAL_UNIT_ASSIGNED_CONTEXT((#25101,#25103,#25104))
REPRESENTATION_CONTEXT('','3D')
);
#25095=(
GEOMETRIC_REPRESENTATION_CONTEXT(3)
GLOBAL_UNCERTAINTY_ASSIGNED_CONTEXT((#24974))
GLOBAL_UNIT_ASSIGNED_CONTEXT((#25101,#25103,#25104))
REPRESENTATION_CONTEXT('','3D')
);
#25096=(
GEOMETRIC_REPRESENTATION_CONTEXT(3)
GLOBAL_UNCERTAINTY_ASSIGNED_CONTEXT((#24975))
GLOBAL_UNIT_ASSIGNED_CONTEXT((#25101,#25103,#25104))
REPRESENTATION_CONTEXT('','3D')
);
#25097=(
GEOMETRIC_REPRESENTATION_CONTEXT(3)
GLOBAL_UNCERTAINTY_ASSIGNED_CONTEXT((#24976))
GLOBAL_UNIT_ASSIGNED_CONTEXT((#25101,#25103,#25104))
REPRESENTATION_CONTEXT('','3D')
);
#25098=(
GEOMETRIC_REPRESENTATION_CONTEXT(3)
GLOBAL_UNCERTAINTY_ASSIGNED_CONTEXT((#24977))
GLOBAL_UNIT_ASSIGNED_CONTEXT((#25101,#25103,#25104))
REPRESENTATION_CONTEXT('','3D')
);
#25099=(
GEOMETRIC_REPRESENTATION_CONTEXT(3)
GLOBAL_UNCERTAINTY_ASSIGNED_CONTEXT((#24978))
GLOBAL_UNIT_ASSIGNED_CONTEXT((#25101,#25103,#25104))
REPRESENTATION_CONTEXT('','3D')
);
#25100=(
GEOMETRIC_REPRESENTATION_CONTEXT(3)
GLOBAL_UNCERTAINTY_ASSIGNED_CONTEXT((#24979))
GLOBAL_UNIT_ASSIGNED_CONTEXT((#25101,#25103,#25104))
REPRESENTATION_CONTEXT('','3D')
);
#25101=(
LENGTH_UNIT()
NAMED_UNIT(*)
SI_UNIT(.CENTI.,.METRE.)
);
#25102=(
LENGTH_UNIT()
NAMED_UNIT(*)
SI_UNIT($,.METRE.)
);
#25103=(
NAMED_UNIT(*)
PLANE_ANGLE_UNIT()
SI_UNIT($,.RADIAN.)
);
#25104=(
NAMED_UNIT(*)
SI_UNIT($,.STERADIAN.)
SOLID_ANGLE_UNIT()
);
#25105=SHAPE_DEFINITION_REPRESENTATION(#25225,#25510);
#25106=SHAPE_DEFINITION_REPRESENTATION(#25226,#25511);
#25107=SHAPE_DEFINITION_REPRESENTATION(#25227,#25512);
#25108=SHAPE_DEFINITION_REPRESENTATION(#25228,#25513);
#25109=SHAPE_DEFINITION_REPRESENTATION(#25229,#25514);
#25110=SHAPE_DEFINITION_REPRESENTATION(#25230,#25515);
#25111=SHAPE_DEFINITION_REPRESENTATION(#25231,#25516);
#25112=SHAPE_DEFINITION_REPRESENTATION(#25232,#25517);
#25113=SHAPE_DEFINITION_REPRESENTATION(#25233,#25518);
#25114=SHAPE_DEFINITION_REPRESENTATION(#25234,#25519);
#25115=SHAPE_DEFINITION_REPRESENTATION(#25235,#25520);
#25116=SHAPE_DEFINITION_REPRESENTATION(#25236,#25521);
#25117=SHAPE_DEFINITION_REPRESENTATION(#25237,#25522);
#25118=SHAPE_DEFINITION_REPRESENTATION(#25238,#25523);
#25119=SHAPE_DEFINITION_REPRESENTATION(#25239,#25524);
#25120=SHAPE_DEFINITION_REPRESENTATION(#25240,#25525);
#25121=SHAPE_DEFINITION_REPRESENTATION(#25241,#25526);
#25122=SHAPE_DEFINITION_REPRESENTATION(#25242,#25527);
#25123=SHAPE_DEFINITION_REPRESENTATION(#25243,#25528);
#25124=SHAPE_DEFINITION_REPRESENTATION(#25244,#25529);
#25125=SHAPE_DEFINITION_REPRESENTATION(#25245,#25530);
#25126=SHAPE_DEFINITION_REPRESENTATION(#25246,#25531);
#25127=SHAPE_DEFINITION_REPRESENTATION(#25247,#25532);
#25128=SHAPE_DEFINITION_REPRESENTATION(#25248,#25533);
#25129=SHAPE_DEFINITION_REPRESENTATION(#25249,#25534);
#25130=SHAPE_DEFINITION_REPRESENTATION(#25250,#25535);
#25131=SHAPE_DEFINITION_REPRESENTATION(#25251,#25536);
#25132=SHAPE_DEFINITION_REPRESENTATION(#25252,#25537);
#25133=SHAPE_DEFINITION_REPRESENTATION(#25253,#25538);
#25134=SHAPE_DEFINITION_REPRESENTATION(#25254,#25539);
#25135=SHAPE_DEFINITION_REPRESENTATION(#25255,#25540);
#25136=SHAPE_DEFINITION_REPRESENTATION(#25256,#25541);
#25137=SHAPE_DEFINITION_REPRESENTATION(#25257,#25542);
#25138=SHAPE_DEFINITION_REPRESENTATION(#25258,#25543);
#25139=SHAPE_DEFINITION_REPRESENTATION(#25259,#25544);
#25140=SHAPE_DEFINITION_REPRESENTATION(#25260,#25545);
#25141=SHAPE_DEFINITION_REPRESENTATION(#25261,#25546);
#25142=SHAPE_DEFINITION_REPRESENTATION(#25262,#25547);
#25143=SHAPE_DEFINITION_REPRESENTATION(#25263,#25548);
#25144=SHAPE_DEFINITION_REPRESENTATION(#25264,#25549);
#25145=SHAPE_DEFINITION_REPRESENTATION(#25265,#25550);
#25146=SHAPE_DEFINITION_REPRESENTATION(#25266,#25551);
#25147=SHAPE_DEFINITION_REPRESENTATION(#25267,#25552);
#25148=SHAPE_DEFINITION_REPRESENTATION(#25268,#25553);
#25149=SHAPE_DEFINITION_REPRESENTATION(#25269,#25554);
#25150=SHAPE_DEFINITION_REPRESENTATION(#25270,#25555);
#25151=SHAPE_DEFINITION_REPRESENTATION(#25271,#25556);
#25152=SHAPE_DEFINITION_REPRESENTATION(#25272,#25557);
#25153=SHAPE_DEFINITION_REPRESENTATION(#25273,#25558);
#25154=SHAPE_DEFINITION_REPRESENTATION(#25274,#25559);
#25155=SHAPE_DEFINITION_REPRESENTATION(#25275,#25560);
#25156=SHAPE_DEFINITION_REPRESENTATION(#25276,#25561);
#25157=SHAPE_DEFINITION_REPRESENTATION(#25277,#25562);
#25158=SHAPE_DEFINITION_REPRESENTATION(#25278,#25563);
#25159=SHAPE_DEFINITION_REPRESENTATION(#25279,#25564);
#25160=SHAPE_DEFINITION_REPRESENTATION(#25280,#25565);
#25161=SHAPE_DEFINITION_REPRESENTATION(#25281,#25566);
#25162=SHAPE_DEFINITION_REPRESENTATION(#25282,#25567);
#25163=SHAPE_DEFINITION_REPRESENTATION(#25283,#25568);
#25164=SHAPE_DEFINITION_REPRESENTATION(#25284,#25569);
#25165=SHAPE_DEFINITION_REPRESENTATION(#25285,#25570);
#25166=SHAPE_DEFINITION_REPRESENTATION(#25288,#25571);
#25167=SHAPE_DEFINITION_REPRESENTATION(#25289,#25572);
#25168=SHAPE_DEFINITION_REPRESENTATION(#25290,#25573);
#25169=SHAPE_DEFINITION_REPRESENTATION(#25291,#25574);
#25170=SHAPE_DEFINITION_REPRESENTATION(#25292,#25575);
#25171=SHAPE_DEFINITION_REPRESENTATION(#25293,#25576);
#25172=SHAPE_DEFINITION_REPRESENTATION(#25294,#25577);
#25173=SHAPE_DEFINITION_REPRESENTATION(#25295,#25578);
#25174=SHAPE_DEFINITION_REPRESENTATION(#25296,#25579);
#25175=SHAPE_DEFINITION_REPRESENTATION(#25297,#25580);
#25176=SHAPE_DEFINITION_REPRESENTATION(#25298,#25581);
#25177=SHAPE_DEFINITION_REPRESENTATION(#25299,#25582);
#25178=SHAPE_DEFINITION_REPRESENTATION(#25300,#25583);
#25179=SHAPE_DEFINITION_REPRESENTATION(#25301,#25584);
#25180=SHAPE_DEFINITION_REPRESENTATION(#25302,#25585);
#25181=SHAPE_DEFINITION_REPRESENTATION(#25303,#25586);
#25182=SHAPE_DEFINITION_REPRESENTATION(#25304,#25587);
#25183=SHAPE_DEFINITION_REPRESENTATION(#25305,#25588);
#25184=SHAPE_DEFINITION_REPRESENTATION(#25306,#25589);
#25185=SHAPE_DEFINITION_REPRESENTATION(#25379,#25590);
#25186=SHAPE_DEFINITION_REPRESENTATION(#25380,#25591);
#25187=SHAPE_DEFINITION_REPRESENTATION(#25381,#25592);
#25188=SHAPE_DEFINITION_REPRESENTATION(#25382,#25593);
#25189=SHAPE_DEFINITION_REPRESENTATION(#25383,#25594);
#25190=SHAPE_DEFINITION_REPRESENTATION(#25384,#25595);
#25191=SHAPE_DEFINITION_REPRESENTATION(#25385,#25596);
#25192=SHAPE_DEFINITION_REPRESENTATION(#25386,#25597);
#25193=SHAPE_DEFINITION_REPRESENTATION(#25387,#25598);
#25194=SHAPE_DEFINITION_REPRESENTATION(#25388,#25599);
#25195=SHAPE_DEFINITION_REPRESENTATION(#25389,#25600);
#25196=SHAPE_DEFINITION_REPRESENTATION(#25390,#25601);
#25197=SHAPE_DEFINITION_REPRESENTATION(#25391,#25602);
#25198=SHAPE_DEFINITION_REPRESENTATION(#25392,#25603);
#25199=SHAPE_DEFINITION_REPRESENTATION(#25393,#25604);
#25200=SHAPE_DEFINITION_REPRESENTATION(#25394,#25605);
#25201=SHAPE_DEFINITION_REPRESENTATION(#25395,#25606);
#25202=SHAPE_DEFINITION_REPRESENTATION(#25396,#25607);
#25203=SHAPE_DEFINITION_REPRESENTATION(#25397,#25608);
#25204=SHAPE_DEFINITION_REPRESENTATION(#25398,#25609);
#25205=SHAPE_DEFINITION_REPRESENTATION(#25399,#25610);
#25206=SHAPE_DEFINITION_REPRESENTATION(#25400,#25611);
#25207=SHAPE_DEFINITION_REPRESENTATION(#25401,#25612);
#25208=SHAPE_DEFINITION_REPRESENTATION(#25402,#25613);
#25209=SHAPE_DEFINITION_REPRESENTATION(#25403,#25614);
#25210=SHAPE_DEFINITION_REPRESENTATION(#25404,#25615);
#25211=SHAPE_DEFINITION_REPRESENTATION(#25405,#25616);
#25212=SHAPE_DEFINITION_REPRESENTATION(#25406,#25617);
#25213=SHAPE_DEFINITION_REPRESENTATION(#25407,#25618);
#25214=SHAPE_DEFINITION_REPRESENTATION(#25408,#25619);
#25215=SHAPE_DEFINITION_REPRESENTATION(#25409,#25620);
#25216=SHAPE_DEFINITION_REPRESENTATION(#25410,#25621);
#25217=SHAPE_DEFINITION_REPRESENTATION(#25411,#25622);
#25218=SHAPE_DEFINITION_REPRESENTATION(#25490,#25623);
#25219=SHAPE_DEFINITION_REPRESENTATION(#25491,#25624);
#25220=SHAPE_DEFINITION_REPRESENTATION(#25492,#25625);
#25221=SHAPE_DEFINITION_REPRESENTATION(#25493,#25626);
#25222=SHAPE_DEFINITION_REPRESENTATION(#25494,#25627);
#25223=SHAPE_DEFINITION_REPRESENTATION(#25495,#25628);
#25224=SHAPE_DEFINITION_REPRESENTATION(#25496,#25629);
#25225=PRODUCT_DEFINITION_SHAPE('',$,#25631);
#25226=PRODUCT_DEFINITION_SHAPE('',$,#25632);
#25227=PRODUCT_DEFINITION_SHAPE('',$,#25633);
#25228=PRODUCT_DEFINITION_SHAPE('',$,#25634);
#25229=PRODUCT_DEFINITION_SHAPE('',$,#25635);
#25230=PRODUCT_DEFINITION_SHAPE('',$,#25636);
#25231=PRODUCT_DEFINITION_SHAPE('',$,#25637);
#25232=PRODUCT_DEFINITION_SHAPE('',$,#25638);
#25233=PRODUCT_DEFINITION_SHAPE('',$,#25639);
#25234=PRODUCT_DEFINITION_SHAPE('',$,#25640);
#25235=PRODUCT_DEFINITION_SHAPE('',$,#25641);
#25236=PRODUCT_DEFINITION_SHAPE('',$,#25642);
#25237=PRODUCT_DEFINITION_SHAPE('',$,#25643);
#25238=PRODUCT_DEFINITION_SHAPE('',$,#25644);
#25239=PRODUCT_DEFINITION_SHAPE('',$,#25645);
#25240=PRODUCT_DEFINITION_SHAPE('',$,#25646);
#25241=PRODUCT_DEFINITION_SHAPE('',$,#25647);
#25242=PRODUCT_DEFINITION_SHAPE('',$,#25648);
#25243=PRODUCT_DEFINITION_SHAPE('',$,#25649);
#25244=PRODUCT_DEFINITION_SHAPE('',$,#25650);
#25245=PRODUCT_DEFINITION_SHAPE('',$,#25651);
#25246=PRODUCT_DEFINITION_SHAPE('',$,#25652);
#25247=PRODUCT_DEFINITION_SHAPE('',$,#25653);
#25248=PRODUCT_DEFINITION_SHAPE('',$,#25654);
#25249=PRODUCT_DEFINITION_SHAPE('',$,#25655);
#25250=PRODUCT_DEFINITION_SHAPE('',$,#25656);
#25251=PRODUCT_DEFINITION_SHAPE('',$,#25657);
#25252=PRODUCT_DEFINITION_SHAPE('',$,#25658);
#25253=PRODUCT_DEFINITION_SHAPE('',$,#25659);
#25254=PRODUCT_DEFINITION_SHAPE('',$,#25660);
#25255=PRODUCT_DEFINITION_SHAPE('',$,#25661);
#25256=PRODUCT_DEFINITION_SHAPE('',$,#25662);
#25257=PRODUCT_DEFINITION_SHAPE('',$,#25663);
#25258=PRODUCT_DEFINITION_SHAPE('',$,#25664);
#25259=PRODUCT_DEFINITION_SHAPE('',$,#25665);
#25260=PRODUCT_DEFINITION_SHAPE('',$,#25666);
#25261=PRODUCT_DEFINITION_SHAPE('',$,#25667);
#25262=PRODUCT_DEFINITION_SHAPE('',$,#25668);
#25263=PRODUCT_DEFINITION_SHAPE('',$,#25669);
#25264=PRODUCT_DEFINITION_SHAPE('',$,#25670);
#25265=PRODUCT_DEFINITION_SHAPE('',$,#25671);
#25266=PRODUCT_DEFINITION_SHAPE('',$,#25672);
#25267=PRODUCT_DEFINITION_SHAPE('',$,#25673);
#25268=PRODUCT_DEFINITION_SHAPE('',$,#25674);
#25269=PRODUCT_DEFINITION_SHAPE('',$,#25675);
#25270=PRODUCT_DEFINITION_SHAPE('',$,#25676);
#25271=PRODUCT_DEFINITION_SHAPE('',$,#25677);
#25272=PRODUCT_DEFINITION_SHAPE('',$,#25678);
#25273=PRODUCT_DEFINITION_SHAPE('',$,#25679);
#25274=PRODUCT_DEFINITION_SHAPE('',$,#25680);
#25275=PRODUCT_DEFINITION_SHAPE('',$,#25681);
#25276=PRODUCT_DEFINITION_SHAPE('',$,#25682);
#25277=PRODUCT_DEFINITION_SHAPE('',$,#25683);
#25278=PRODUCT_DEFINITION_SHAPE('',$,#25684);
#25279=PRODUCT_DEFINITION_SHAPE('',$,#25685);
#25280=PRODUCT_DEFINITION_SHAPE('',$,#25686);
#25281=PRODUCT_DEFINITION_SHAPE('',$,#25687);
#25282=PRODUCT_DEFINITION_SHAPE('',$,#25688);
#25283=PRODUCT_DEFINITION_SHAPE('',$,#25689);
#25284=PRODUCT_DEFINITION_SHAPE('',$,#25690);
#25285=PRODUCT_DEFINITION_SHAPE('',$,#25691);
#25286=PRODUCT_DEFINITION_SHAPE($,$,#532);
#25287=PRODUCT_DEFINITION_SHAPE($,$,#533);
#25288=PRODUCT_DEFINITION_SHAPE('',$,#25692);
#25289=PRODUCT_DEFINITION_SHAPE('',$,#25693);
#25290=PRODUCT_DEFINITION_SHAPE('',$,#25694);
#25291=PRODUCT_DEFINITION_SHAPE('',$,#25695);
#25292=PRODUCT_DEFINITION_SHAPE('',$,#25696);
#25293=PRODUCT_DEFINITION_SHAPE('',$,#25697);
#25294=PRODUCT_DEFINITION_SHAPE('',$,#25698);
#25295=PRODUCT_DEFINITION_SHAPE('',$,#25699);
#25296=PRODUCT_DEFINITION_SHAPE('',$,#25700);
#25297=PRODUCT_DEFINITION_SHAPE('',$,#25701);
#25298=PRODUCT_DEFINITION_SHAPE('',$,#25702);
#25299=PRODUCT_DEFINITION_SHAPE('',$,#25703);
#25300=PRODUCT_DEFINITION_SHAPE('',$,#25704);
#25301=PRODUCT_DEFINITION_SHAPE('',$,#25705);
#25302=PRODUCT_DEFINITION_SHAPE('',$,#25706);
#25303=PRODUCT_DEFINITION_SHAPE('',$,#25707);
#25304=PRODUCT_DEFINITION_SHAPE('',$,#25708);
#25305=PRODUCT_DEFINITION_SHAPE('',$,#25709);
#25306=PRODUCT_DEFINITION_SHAPE('',$,#25710);
#25307=PRODUCT_DEFINITION_SHAPE($,$,#534);
#25308=PRODUCT_DEFINITION_SHAPE($,$,#535);
#25309=PRODUCT_DEFINITION_SHAPE($,$,#536);
#25310=PRODUCT_DEFINITION_SHAPE($,$,#537);
#25311=PRODUCT_DEFINITION_SHAPE($,$,#538);
#25312=PRODUCT_DEFINITION_SHAPE($,$,#539);
#25313=PRODUCT_DEFINITION_SHAPE($,$,#540);
#25314=PRODUCT_DEFINITION_SHAPE($,$,#541);
#25315=PRODUCT_DEFINITION_SHAPE($,$,#542);
#25316=PRODUCT_DEFINITION_SHAPE($,$,#543);
#25317=PRODUCT_DEFINITION_SHAPE($,$,#544);
#25318=PRODUCT_DEFINITION_SHAPE($,$,#545);
#25319=PRODUCT_DEFINITION_SHAPE($,$,#546);
#25320=PRODUCT_DEFINITION_SHAPE($,$,#547);
#25321=PRODUCT_DEFINITION_SHAPE($,$,#548);
#25322=PRODUCT_DEFINITION_SHAPE($,$,#549);
#25323=PRODUCT_DEFINITION_SHAPE($,$,#550);
#25324=PRODUCT_DEFINITION_SHAPE($,$,#551);
#25325=PRODUCT_DEFINITION_SHAPE($,$,#552);
#25326=PRODUCT_DEFINITION_SHAPE($,$,#553);
#25327=PRODUCT_DEFINITION_SHAPE($,$,#554);
#25328=PRODUCT_DEFINITION_SHAPE($,$,#555);
#25329=PRODUCT_DEFINITION_SHAPE($,$,#556);
#25330=PRODUCT_DEFINITION_SHAPE($,$,#557);
#25331=PRODUCT_DEFINITION_SHAPE($,$,#558);
#25332=PRODUCT_DEFINITION_SHAPE($,$,#559);
#25333=PRODUCT_DEFINITION_SHAPE($,$,#560);
#25334=PRODUCT_DEFINITION_SHAPE($,$,#561);
#25335=PRODUCT_DEFINITION_SHAPE($,$,#562);
#25336=PRODUCT_DEFINITION_SHAPE($,$,#563);
#25337=PRODUCT_DEFINITION_SHAPE($,$,#564);
#25338=PRODUCT_DEFINITION_SHAPE($,$,#565);
#25339=PRODUCT_DEFINITION_SHAPE($,$,#566);
#25340=PRODUCT_DEFINITION_SHAPE($,$,#567);
#25341=PRODUCT_DEFINITION_SHAPE($,$,#568);
#25342=PRODUCT_DEFINITION_SHAPE($,$,#569);
#25343=PRODUCT_DEFINITION_SHAPE($,$,#570);
#25344=PRODUCT_DEFINITION_SHAPE($,$,#571);
#25345=PRODUCT_DEFINITION_SHAPE($,$,#572);
#25346=PRODUCT_DEFINITION_SHAPE($,$,#573);
#25347=PRODUCT_DEFINITION_SHAPE($,$,#574);
#25348=PRODUCT_DEFINITION_SHAPE($,$,#575);
#25349=PRODUCT_DEFINITION_SHAPE($,$,#576);
#25350=PRODUCT_DEFINITION_SHAPE($,$,#577);
#25351=PRODUCT_DEFINITION_SHAPE($,$,#578);
#25352=PRODUCT_DEFINITION_SHAPE($,$,#579);
#25353=PRODUCT_DEFINITION_SHAPE($,$,#580);
#25354=PRODUCT_DEFINITION_SHAPE($,$,#581);
#25355=PRODUCT_DEFINITION_SHAPE($,$,#582);
#25356=PRODUCT_DEFINITION_SHAPE($,$,#583);
#25357=PRODUCT_DEFINITION_SHAPE($,$,#584);
#25358=PRODUCT_DEFINITION_SHAPE($,$,#585);
#25359=PRODUCT_DEFINITION_SHAPE($,$,#586);
#25360=PRODUCT_DEFINITION_SHAPE($,$,#587);
#25361=PRODUCT_DEFINITION_SHAPE($,$,#588);
#25362=PRODUCT_DEFINITION_SHAPE($,$,#589);
#25363=PRODUCT_DEFINITION_SHAPE($,$,#590);
#25364=PRODUCT_DEFINITION_SHAPE($,$,#591);
#25365=PRODUCT_DEFINITION_SHAPE($,$,#592);
#25366=PRODUCT_DEFINITION_SHAPE($,$,#593);
#25367=PRODUCT_DEFINITION_SHAPE($,$,#594);
#25368=PRODUCT_DEFINITION_SHAPE($,$,#595);
#25369=PRODUCT_DEFINITION_SHAPE($,$,#596);
#25370=PRODUCT_DEFINITION_SHAPE($,$,#597);
#25371=PRODUCT_DEFINITION_SHAPE($,$,#598);
#25372=PRODUCT_DEFINITION_SHAPE($,$,#599);
#25373=PRODUCT_DEFINITION_SHAPE($,$,#600);
#25374=PRODUCT_DEFINITION_SHAPE($,$,#601);
#25375=PRODUCT_DEFINITION_SHAPE($,$,#602);
#25376=PRODUCT_DEFINITION_SHAPE($,$,#603);
#25377=PRODUCT_DEFINITION_SHAPE($,$,#604);
#25378=PRODUCT_DEFINITION_SHAPE($,$,#605);
#25379=PRODUCT_DEFINITION_SHAPE('',$,#25711);
#25380=PRODUCT_DEFINITION_SHAPE('',$,#25712);
#25381=PRODUCT_DEFINITION_SHAPE('',$,#25713);
#25382=PRODUCT_DEFINITION_SHAPE('',$,#25714);
#25383=PRODUCT_DEFINITION_SHAPE('',$,#25715);
#25384=PRODUCT_DEFINITION_SHAPE('',$,#25716);
#25385=PRODUCT_DEFINITION_SHAPE('',$,#25717);
#25386=PRODUCT_DEFINITION_SHAPE('',$,#25718);
#25387=PRODUCT_DEFINITION_SHAPE('',$,#25719);
#25388=PRODUCT_DEFINITION_SHAPE('',$,#25720);
#25389=PRODUCT_DEFINITION_SHAPE('',$,#25721);
#25390=PRODUCT_DEFINITION_SHAPE('',$,#25722);
#25391=PRODUCT_DEFINITION_SHAPE('',$,#25723);
#25392=PRODUCT_DEFINITION_SHAPE('',$,#25724);
#25393=PRODUCT_DEFINITION_SHAPE('',$,#25725);
#25394=PRODUCT_DEFINITION_SHAPE('',$,#25726);
#25395=PRODUCT_DEFINITION_SHAPE('',$,#25727);
#25396=PRODUCT_DEFINITION_SHAPE('',$,#25728);
#25397=PRODUCT_DEFINITION_SHAPE('',$,#25729);
#25398=PRODUCT_DEFINITION_SHAPE('',$,#25730);
#25399=PRODUCT_DEFINITION_SHAPE('',$,#25731);
#25400=PRODUCT_DEFINITION_SHAPE('',$,#25732);
#25401=PRODUCT_DEFINITION_SHAPE('',$,#25733);
#25402=PRODUCT_DEFINITION_SHAPE('',$,#25734);
#25403=PRODUCT_DEFINITION_SHAPE('',$,#25735);
#25404=PRODUCT_DEFINITION_SHAPE('',$,#25736);
#25405=PRODUCT_DEFINITION_SHAPE('',$,#25737);
#25406=PRODUCT_DEFINITION_SHAPE('',$,#25738);
#25407=PRODUCT_DEFINITION_SHAPE('',$,#25739);
#25408=PRODUCT_DEFINITION_SHAPE('',$,#25740);
#25409=PRODUCT_DEFINITION_SHAPE('',$,#25741);
#25410=PRODUCT_DEFINITION_SHAPE('',$,#25742);
#25411=PRODUCT_DEFINITION_SHAPE('',$,#25743);
#25412=PRODUCT_DEFINITION_SHAPE($,$,#606);
#25413=PRODUCT_DEFINITION_SHAPE($,$,#607);
#25414=PRODUCT_DEFINITION_SHAPE($,$,#608);
#25415=PRODUCT_DEFINITION_SHAPE($,$,#609);
#25416=PRODUCT_DEFINITION_SHAPE($,$,#610);
#25417=PRODUCT_DEFINITION_SHAPE($,$,#611);
#25418=PRODUCT_DEFINITION_SHAPE($,$,#612);
#25419=PRODUCT_DEFINITION_SHAPE($,$,#613);
#25420=PRODUCT_DEFINITION_SHAPE($,$,#614);
#25421=PRODUCT_DEFINITION_SHAPE($,$,#615);
#25422=PRODUCT_DEFINITION_SHAPE($,$,#616);
#25423=PRODUCT_DEFINITION_SHAPE($,$,#617);
#25424=PRODUCT_DEFINITION_SHAPE($,$,#618);
#25425=PRODUCT_DEFINITION_SHAPE($,$,#619);
#25426=PRODUCT_DEFINITION_SHAPE($,$,#620);
#25427=PRODUCT_DEFINITION_SHAPE($,$,#621);
#25428=PRODUCT_DEFINITION_SHAPE($,$,#622);
#25429=PRODUCT_DEFINITION_SHAPE($,$,#623);
#25430=PRODUCT_DEFINITION_SHAPE($,$,#624);
#25431=PRODUCT_DEFINITION_SHAPE($,$,#625);
#25432=PRODUCT_DEFINITION_SHAPE($,$,#626);
#25433=PRODUCT_DEFINITION_SHAPE($,$,#627);
#25434=PRODUCT_DEFINITION_SHAPE($,$,#628);
#25435=PRODUCT_DEFINITION_SHAPE($,$,#629);
#25436=PRODUCT_DEFINITION_SHAPE($,$,#630);
#25437=PRODUCT_DEFINITION_SHAPE($,$,#631);
#25438=PRODUCT_DEFINITION_SHAPE($,$,#632);
#25439=PRODUCT_DEFINITION_SHAPE($,$,#633);
#25440=PRODUCT_DEFINITION_SHAPE($,$,#634);
#25441=PRODUCT_DEFINITION_SHAPE($,$,#635);
#25442=PRODUCT_DEFINITION_SHAPE($,$,#636);
#25443=PRODUCT_DEFINITION_SHAPE($,$,#637);
#25444=PRODUCT_DEFINITION_SHAPE($,$,#638);
#25445=PRODUCT_DEFINITION_SHAPE($,$,#639);
#25446=PRODUCT_DEFINITION_SHAPE($,$,#640);
#25447=PRODUCT_DEFINITION_SHAPE($,$,#641);
#25448=PRODUCT_DEFINITION_SHAPE($,$,#642);
#25449=PRODUCT_DEFINITION_SHAPE($,$,#643);
#25450=PRODUCT_DEFINITION_SHAPE($,$,#644);
#25451=PRODUCT_DEFINITION_SHAPE($,$,#645);
#25452=PRODUCT_DEFINITION_SHAPE($,$,#646);
#25453=PRODUCT_DEFINITION_SHAPE($,$,#647);
#25454=PRODUCT_DEFINITION_SHAPE($,$,#648);
#25455=PRODUCT_DEFINITION_SHAPE($,$,#649);
#25456=PRODUCT_DEFINITION_SHAPE($,$,#650);
#25457=PRODUCT_DEFINITION_SHAPE($,$,#651);
#25458=PRODUCT_DEFINITION_SHAPE($,$,#652);
#25459=PRODUCT_DEFINITION_SHAPE($,$,#653);
#25460=PRODUCT_DEFINITION_SHAPE($,$,#654);
#25461=PRODUCT_DEFINITION_SHAPE($,$,#655);
#25462=PRODUCT_DEFINITION_SHAPE($,$,#656);
#25463=PRODUCT_DEFINITION_SHAPE($,$,#657);
#25464=PRODUCT_DEFINITION_SHAPE($,$,#658);
#25465=PRODUCT_DEFINITION_SHAPE($,$,#659);
#25466=PRODUCT_DEFINITION_SHAPE($,$,#660);
#25467=PRODUCT_DEFINITION_SHAPE($,$,#661);
#25468=PRODUCT_DEFINITION_SHAPE($,$,#662);
#25469=PRODUCT_DEFINITION_SHAPE($,$,#663);
#25470=PRODUCT_DEFINITION_SHAPE($,$,#664);
#25471=PRODUCT_DEFINITION_SHAPE($,$,#665);
#25472=PRODUCT_DEFINITION_SHAPE($,$,#666);
#25473=PRODUCT_DEFINITION_SHAPE($,$,#667);
#25474=PRODUCT_DEFINITION_SHAPE($,$,#668);
#25475=PRODUCT_DEFINITION_SHAPE($,$,#669);
#25476=PRODUCT_DEFINITION_SHAPE($,$,#670);
#25477=PRODUCT_DEFINITION_SHAPE($,$,#671);
#25478=PRODUCT_DEFINITION_SHAPE($,$,#672);
#25479=PRODUCT_DEFINITION_SHAPE($,$,#673);
#25480=PRODUCT_DEFINITION_SHAPE($,$,#674);
#25481=PRODUCT_DEFINITION_SHAPE($,$,#675);
#25482=PRODUCT_DEFINITION_SHAPE($,$,#676);
#25483=PRODUCT_DEFINITION_SHAPE($,$,#677);
#25484=PRODUCT_DEFINITION_SHAPE($,$,#678);
#25485=PRODUCT_DEFINITION_SHAPE($,$,#679);
#25486=PRODUCT_DEFINITION_SHAPE($,$,#680);
#25487=PRODUCT_DEFINITION_SHAPE($,$,#681);
#25488=PRODUCT_DEFINITION_SHAPE($,$,#682);
#25489=PRODUCT_DEFINITION_SHAPE($,$,#683);
#25490=PRODUCT_DEFINITION_SHAPE('',$,#25744);
#25491=PRODUCT_DEFINITION_SHAPE('',$,#25745);
#25492=PRODUCT_DEFINITION_SHAPE('',$,#25746);
#25493=PRODUCT_DEFINITION_SHAPE('',$,#25747);
#25494=PRODUCT_DEFINITION_SHAPE('',$,#25748);
#25495=PRODUCT_DEFINITION_SHAPE('',$,#25749);
#25496=PRODUCT_DEFINITION_SHAPE('',$,#25750);
#25497=PRODUCT_DEFINITION_SHAPE($,$,#684);
#25498=PRODUCT_DEFINITION_SHAPE($,$,#685);
#25499=PRODUCT_DEFINITION_SHAPE($,$,#686);
#25500=PRODUCT_DEFINITION_SHAPE($,$,#687);
#25501=PRODUCT_DEFINITION_SHAPE($,$,#688);
#25502=PRODUCT_DEFINITION_SHAPE($,$,#689);
#25503=PRODUCT_DEFINITION_SHAPE($,$,#690);
#25504=PRODUCT_DEFINITION_SHAPE($,$,#691);
#25505=PRODUCT_DEFINITION_SHAPE($,$,#692);
#25506=PRODUCT_DEFINITION_SHAPE($,$,#693);
#25507=PRODUCT_DEFINITION_SHAPE($,$,#694);
#25508=PRODUCT_DEFINITION_SHAPE($,$,#695);
#25509=PRODUCT_DEFINITION_SHAPE($,$,#696);
#25510=SHAPE_REPRESENTATION('',(#14585,#16460,#16461,#16462,#16463,#16464,
#16465,#16466),#24980);
#25511=SHAPE_REPRESENTATION('',(#14586,#16309,#16310,#16311,#16312,#16313,
#16314,#16315,#16316,#16317,#16318,#16319,#16320,#16321,#16322,#16323,#16324,
#16325,#16326,#16327,#16328,#16329,#16330,#16331,#16332,#16333,#16334,#16335,
#16336,#16337,#16338,#16339,#16340,#16341,#16342,#16343,#16344,#16345,#16346,
#16347,#16348,#16349,#16350,#16351,#16352,#16353),#24981);
#25512=SHAPE_REPRESENTATION('',(#14587),#24982);
#25513=SHAPE_REPRESENTATION('',(#14618),#24983);
#25514=SHAPE_REPRESENTATION('',(#14625),#24984);
#25515=SHAPE_REPRESENTATION('',(#14632),#24985);
#25516=SHAPE_REPRESENTATION('',(#14679),#24986);
#25517=SHAPE_REPRESENTATION('',(#14704),#24987);
#25518=SHAPE_REPRESENTATION('',(#14729),#24988);
#25519=SHAPE_REPRESENTATION('',(#14773),#24989);
#25520=SHAPE_REPRESENTATION('',(#14798),#24990);
#25521=SHAPE_REPRESENTATION('',(#14823),#24991);
#25522=SHAPE_REPRESENTATION('',(#14829),#24992);
#25523=SHAPE_REPRESENTATION('',(#14835),#24993);
#25524=SHAPE_REPRESENTATION('',(#14849),#24994);
#25525=SHAPE_REPRESENTATION('',(#14858),#24995);
#25526=SHAPE_REPRESENTATION('',(#14867),#24996);
#25527=SHAPE_REPRESENTATION('',(#14876),#24997);
#25528=SHAPE_REPRESENTATION('',(#14885),#24998);
#25529=SHAPE_REPRESENTATION('',(#14894),#24999);
#25530=SHAPE_REPRESENTATION('',(#14918,#15699,#15700,#15701,#15702,#15703,
#15704,#15705,#15706,#15707,#15708,#15709,#15710,#15711,#15712,#15713,#15714,
#15715,#15716,#15717,#15718,#15719,#15720),#25000);
#25531=SHAPE_REPRESENTATION('',(#14919),#25001);
#25532=SHAPE_REPRESENTATION('',(#14950),#25002);
#25533=SHAPE_REPRESENTATION('',(#14983),#25003);
#25534=SHAPE_REPRESENTATION('',(#15012),#25004);
#25535=SHAPE_REPRESENTATION('',(#15018),#25005);
#25536=SHAPE_REPRESENTATION('',(#15024),#25006);
#25537=SHAPE_REPRESENTATION('',(#15038),#25007);
#25538=SHAPE_REPRESENTATION('',(#15047),#25008);
#25539=SHAPE_REPRESENTATION('',(#15056),#25009);
#25540=SHAPE_REPRESENTATION('',(#15065),#25010);
#25541=SHAPE_REPRESENTATION('',(#15074),#25011);
#25542=SHAPE_REPRESENTATION('',(#15083),#25012);
#25543=SHAPE_REPRESENTATION('',(#15092),#25013);
#25544=SHAPE_REPRESENTATION('',(#15118,#15721,#15722,#15723,#15724,#15725,
#15726,#15727,#15728,#15729,#15730,#15731,#15732,#15733,#15734,#15735,#15736),
#25014);
#25545=SHAPE_REPRESENTATION('',(#15119),#25015);
#25546=SHAPE_REPRESENTATION('',(#15135),#25016);
#25547=SHAPE_REPRESENTATION('',(#15159),#25017);
#25548=SHAPE_REPRESENTATION('',(#15183),#25018);
#25549=SHAPE_REPRESENTATION('',(#15200),#25019);
#25550=SHAPE_REPRESENTATION('',(#15214),#25020);
#25551=SHAPE_REPRESENTATION('',(#15223),#25021);
#25552=SHAPE_REPRESENTATION('',(#15232),#25022);
#25553=SHAPE_REPRESENTATION('',(#15241),#25023);
#25554=SHAPE_REPRESENTATION('',(#15250),#25024);
#25555=SHAPE_REPRESENTATION('',(#15259),#25025);
#25556=SHAPE_REPRESENTATION('',(#15268,#15737,#15738,#15739,#15740,#15741,
#15742,#15743,#15744,#15745,#15746,#15747,#15748,#15749,#15750,#15751,#15752),
#25026);
#25557=SHAPE_REPRESENTATION('',(#15269),#25027);
#25558=SHAPE_REPRESENTATION('',(#15285),#25028);
#25559=SHAPE_REPRESENTATION('',(#15309),#25029);
#25560=SHAPE_REPRESENTATION('',(#15333),#25030);
#25561=SHAPE_REPRESENTATION('',(#15350),#25031);
#25562=SHAPE_REPRESENTATION('',(#15364),#25032);
#25563=SHAPE_REPRESENTATION('',(#15373),#25033);
#25564=SHAPE_REPRESENTATION('',(#15382),#25034);
#25565=SHAPE_REPRESENTATION('',(#15391),#25035);
#25566=SHAPE_REPRESENTATION('',(#15400),#25036);
#25567=SHAPE_REPRESENTATION('',(#15409),#25037);
#25568=SHAPE_REPRESENTATION('',(#15418,#15468,#15469),#25038);
#25569=SHAPE_REPRESENTATION('',(#15419),#25039);
#25570=SHAPE_REPRESENTATION('',(#15451),#25040);
#25571=SHAPE_REPRESENTATION('',(#15470),#25041);
#25572=SHAPE_REPRESENTATION('',(#15485,#15753,#15754,#15755,#15756,#15757,
#15758,#15759,#15760,#15761,#15762,#15763,#15764,#15765,#15766,#15767,#15768,
#15769,#15770),#25042);
#25573=SHAPE_REPRESENTATION('',(#15486),#25043);
#25574=SHAPE_REPRESENTATION('',(#15514),#25044);
#25575=SHAPE_REPRESENTATION('',(#15523),#25045);
#25576=SHAPE_REPRESENTATION('',(#15532),#25046);
#25577=SHAPE_REPRESENTATION('',(#15541),#25047);
#25578=SHAPE_REPRESENTATION('',(#15569),#25048);
#25579=SHAPE_REPRESENTATION('',(#15578),#25049);
#25580=SHAPE_REPRESENTATION('',(#15587),#25050);
#25581=SHAPE_REPRESENTATION('',(#15596),#25051);
#25582=SHAPE_REPRESENTATION('',(#15610),#25052);
#25583=SHAPE_REPRESENTATION('',(#15619),#25053);
#25584=SHAPE_REPRESENTATION('',(#15628),#25054);
#25585=SHAPE_REPRESENTATION('',(#15637),#25055);
#25586=SHAPE_REPRESENTATION('',(#15646),#25056);
#25587=SHAPE_REPRESENTATION('',(#15655),#25057);
#25588=SHAPE_REPRESENTATION('',(#15664),#25058);
#25589=SHAPE_REPRESENTATION('',(#15673),#25059);
#25590=SHAPE_REPRESENTATION('',(#15771,#16354,#16355,#16356,#16357,#16358,
#16359,#16360,#16361,#16362,#16363,#16364,#16365,#16366,#16367,#16368,#16369,
#16370,#16371,#16372,#16373,#16374,#16375,#16376,#16377,#16378,#16379,#16380,
#16381),#25060);
#25591=SHAPE_REPRESENTATION('',(#15772),#25061);
#25592=SHAPE_REPRESENTATION('',(#15812),#25062);
#25593=SHAPE_REPRESENTATION('',(#15821),#25063);
#25594=SHAPE_REPRESENTATION('',(#15830),#25064);
#25595=SHAPE_REPRESENTATION('',(#15851),#25065);
#25596=SHAPE_REPRESENTATION('',(#15861),#25066);
#25597=SHAPE_REPRESENTATION('',(#15871),#25067);
#25598=SHAPE_REPRESENTATION('',(#15881),#25068);
#25599=SHAPE_REPRESENTATION('',(#15891),#25069);
#25600=SHAPE_REPRESENTATION('',(#15912),#25070);
#25601=SHAPE_REPRESENTATION('',(#15922),#25071);
#25602=SHAPE_REPRESENTATION('',(#15932),#25072);
#25603=SHAPE_REPRESENTATION('',(#15942),#25073);
#25604=SHAPE_REPRESENTATION('',(#15952),#25074);
#25605=SHAPE_REPRESENTATION('',(#15992),#25075);
#25606=SHAPE_REPRESENTATION('',(#16001),#25076);
#25607=SHAPE_REPRESENTATION('',(#16010),#25077);
#25608=SHAPE_REPRESENTATION('',(#16031),#25078);
#25609=SHAPE_REPRESENTATION('',(#16041),#25079);
#25610=SHAPE_REPRESENTATION('',(#16051),#25080);
#25611=SHAPE_REPRESENTATION('',(#16061),#25081);
#25612=SHAPE_REPRESENTATION('',(#16071),#25082);
#25613=SHAPE_REPRESENTATION('',(#16092),#25083);
#25614=SHAPE_REPRESENTATION('',(#16102),#25084);
#25615=SHAPE_REPRESENTATION('',(#16112),#25085);
#25616=SHAPE_REPRESENTATION('',(#16122),#25086);
#25617=SHAPE_REPRESENTATION('',(#16132,#16304,#16305,#16306,#16307,#16308),
#25087);
#25618=SHAPE_REPRESENTATION('',(#16133),#25088);
#25619=SHAPE_REPRESENTATION('',(#16153),#25089);
#25620=SHAPE_REPRESENTATION('',(#16173),#25090);
#25621=SHAPE_REPRESENTATION('',(#16188),#25091);
#25622=SHAPE_REPRESENTATION('',(#16287),#25092);
#25623=SHAPE_REPRESENTATION('',(#16382,#16454,#16455,#16456,#16457,#16458,
#16459),#25093);
#25624=SHAPE_REPRESENTATION('',(#16383),#25094);
#25625=SHAPE_REPRESENTATION('',(#16405),#25095);
#25626=SHAPE_REPRESENTATION('',(#16414),#25096);
#25627=SHAPE_REPRESENTATION('',(#16423),#25097);
#25628=SHAPE_REPRESENTATION('',(#16432),#25098);
#25629=SHAPE_REPRESENTATION('',(#16441),#25099);
#25630=PRODUCT_DEFINITION_CONTEXT('part definition',#25992,'design');
#25631=PRODUCT_DEFINITION('PAT-091',
'PAT-091',#25751,#25630);
#25632=PRODUCT_DEFINITION('Base and lower guides',
'Base and lower guides',#25752,#25630);
#25633=PRODUCT_DEFINITION('Base plate','Base plate',#25753,#25630);
#25634=PRODUCT_DEFINITION('Base foot','Base foot',#25754,#25630);
#25635=PRODUCT_DEFINITION('Base foot (1)','Base foot (1)',#25755,#25630);
#25636=PRODUCT_DEFINITION('Lower pivot support','Lower pivot support',#25756,
#25630);
#25637=PRODUCT_DEFINITION('Screw bearing cap','Screw bearing cap',#25757,
#25630);
#25638=PRODUCT_DEFINITION('Screw bearing cap (1)','Screw bearing cap (1)',
#25758,#25630);
#25639=PRODUCT_DEFINITION('Lower screw support','Lower screw support',#25759,
#25630);
#25640=PRODUCT_DEFINITION('Screw bearing cap (2)','Screw bearing cap (2)',
#25760,#25630);
#25641=PRODUCT_DEFINITION('Screw bearing cap (3)','Screw bearing cap (3)',
#25761,#25630);
#25642=PRODUCT_DEFINITION('Guide shaft','Guide shaft',#25762,#25630);
#25643=PRODUCT_DEFINITION('Guide shaft (1)','Guide shaft (1)',#25763,#25630);
#25644=PRODUCT_DEFINITION('Pivot axle 140 mm','Pivot axle 140 mm',#25764,
#25630);
#25645=PRODUCT_DEFINITION('Axle end keeper','Axle end keeper',#25765,#25630);
#25646=PRODUCT_DEFINITION('Axle end keeper (1)','Axle end keeper (1)',#25766,
#25630);
#25647=PRODUCT_DEFINITION('Axle distance sleeve 5 mm',
'Axle distance sleeve 5 mm',#25767,#25630);
#25648=PRODUCT_DEFINITION('Axle distance sleeve 10 mm',
'Axle distance sleeve 10 mm',#25768,#25630);
#25649=PRODUCT_DEFINITION('Axle distance sleeve 5 mm (1)',
'Axle distance sleeve 5 mm (1)',#25769,#25630);
#25650=PRODUCT_DEFINITION('M4x10 Cap Screw','M4x10 Cap Screw',#25770,#25630);
#25651=PRODUCT_DEFINITION('Top and upper guides','Top and upper guides',
#25771,#25630);
#25652=PRODUCT_DEFINITION('Top plate','Top plate',#25772,#25630);
#25653=PRODUCT_DEFINITION('Upper fixed end support',
'Upper fixed end support',#25773,#25630);
#25654=PRODUCT_DEFINITION('Upper sliding end support',
'Upper sliding end support',#25774,#25630);
#25655=PRODUCT_DEFINITION('Guide shaft (2)','Guide shaft (2)',#25775,#25630);
#25656=PRODUCT_DEFINITION('Guide shaft (3)','Guide shaft (3)',#25776,#25630);
#25657=PRODUCT_DEFINITION('Pivot axle 145 mm','Pivot axle 145 mm',#25777,
#25630);
#25658=PRODUCT_DEFINITION('Axle end keeper (2)','Axle end keeper (2)',#25778,
#25630);
#25659=PRODUCT_DEFINITION('Axle end keeper (3)','Axle end keeper (3)',#25779,
#25630);
#25660=PRODUCT_DEFINITION('Axle distance sleeve 5 mm (2)',
'Axle distance sleeve 5 mm (2)',#25780,#25630);
#25661=PRODUCT_DEFINITION('Axle distance sleeve 5 mm (3)',
'Axle distance sleeve 5 mm (3)',#25781,#25630);
#25662=PRODUCT_DEFINITION('Axle distance sleeve 30 mm',
'Axle distance sleeve 30 mm',#25782,#25630);
#25663=PRODUCT_DEFINITION('Axle distance sleeve 5 mm (4)',
'Axle distance sleeve 5 mm (4)',#25783,#25630);
#25664=PRODUCT_DEFINITION('Cap Screw - M5x20','Cap Screw - M5x20',#25784,
#25630);
#25665=PRODUCT_DEFINITION('Lower sliding pivot','Lower sliding pivot',#25785,
#25630);
#25666=PRODUCT_DEFINITION('Lower nut carriage','Lower nut carriage',#25786,
#25630);
#25667=PRODUCT_DEFINITION('Linear bearing keeper',
'Linear bearing keeper',#25787,#25630);
#25668=PRODUCT_DEFINITION('Linear bearing keeper (1)',
'Linear bearing keeper (1)',#25788,#25630);
#25669=PRODUCT_DEFINITION('Sliding pivot crosshead',
'Sliding pivot crosshead',#25789,#25630);
#25670=PRODUCT_DEFINITION('Pivot axle 145 mm (1)','Pivot axle 145 mm (1)',
#25790,#25630);
#25671=PRODUCT_DEFINITION('Axle end keeper (4)','Axle end keeper (4)',#25791,
#25630);
#25672=PRODUCT_DEFINITION('Axle end keeper (5)','Axle end keeper (5)',#25792,
#25630);
#25673=PRODUCT_DEFINITION('Axle distance sleeve 5 mm (5)',
'Axle distance sleeve 5 mm (5)',#25793,#25630);
#25674=PRODUCT_DEFINITION('Axle distance sleeve 10 mm (1)',
'Axle distance sleeve 10 mm (1)',#25794,#25630);
#25675=PRODUCT_DEFINITION('Axle distance sleeve 35 mm',
'Axle distance sleeve 35 mm',#25795,#25630);
#25676=PRODUCT_DEFINITION('Axle distance sleeve 5 mm (6)',
'Axle distance sleeve 5 mm (6)',#25796,#25630);
#25677=PRODUCT_DEFINITION('Upper sliding pivot','Upper sliding pivot',#25797,
#25630);
#25678=PRODUCT_DEFINITION('Upper sliding carriage',
'Upper sliding carriage',#25798,#25630);
#25679=PRODUCT_DEFINITION('Linear bearing keeper (2)',
'Linear bearing keeper (2)',#25799,#25630);
#25680=PRODUCT_DEFINITION('Linear bearing keeper (3)',
'Linear bearing keeper (3)',#25800,#25630);
#25681=PRODUCT_DEFINITION('Sliding pivot crosshead (1)',
'Sliding pivot crosshead (1)',#25801,#25630);
#25682=PRODUCT_DEFINITION('Pivot axle 140 mm (1)','Pivot axle 140 mm (1)',
#25802,#25630);
#25683=PRODUCT_DEFINITION('Axle end keeper (6)','Axle end keeper (6)',#25803,
#25630);
#25684=PRODUCT_DEFINITION('Axle end keeper (7)','Axle end keeper (7)',#25804,
#25630);
#25685=PRODUCT_DEFINITION('Axle distance sleeve 5 mm (7)',
'Axle distance sleeve 5 mm (7)',#25805,#25630);
#25686=PRODUCT_DEFINITION('Axle distance sleeve 25 mm',
'Axle distance sleeve 25 mm',#25806,#25630);
#25687=PRODUCT_DEFINITION('Axle distance sleeve 15 mm',
'Axle distance sleeve 15 mm',#25807,#25630);
#25688=PRODUCT_DEFINITION('Axle distance sleeve 5 mm (8)',
'Axle distance sleeve 5 mm (8)',#25808,#25630);
#25689=PRODUCT_DEFINITION('Linear Ball Bushing - 12 x 21 x 30 mm',
'Linear Ball Bushing - 12 x 21 x 30 mm',#25809,#25630);
#25690=PRODUCT_DEFINITION('Steel sleeve','Steel sleeve',#25810,#25630);
#25691=PRODUCT_DEFINITION('Ball retainer (plastic)',
'Ball retainer (plastic)',#25811,#25630);
#25692=PRODUCT_DEFINITION('M4x4 collar screw','M4x4 collar screw',#25812,
#25630);
#25693=PRODUCT_DEFINITION('Rising arms','Rising arms',#25813,#25630);
#25694=PRODUCT_DEFINITION('Rising arm','Rising arm',#25814,#25630);
#25695=PRODUCT_DEFINITION('Plain pivot bush','Plain pivot bush',#25815,
#25630);
#25696=PRODUCT_DEFINITION('Plain pivot bush (1)','Plain pivot bush (1)',#25816,
#25630);
#25697=PRODUCT_DEFINITION('Plain pivot bush (2)','Plain pivot bush (2)',#25817,
#25630);
#25698=PRODUCT_DEFINITION('Rising arm (1)','Rising arm (1)',#25818,#25630);
#25699=PRODUCT_DEFINITION('Plain pivot bush (3)','Plain pivot bush (3)',#25819,
#25630);
#25700=PRODUCT_DEFINITION('Plain pivot bush (4)','Plain pivot bush (4)',#25820,
#25630);
#25701=PRODUCT_DEFINITION('Plain pivot bush (5)','Plain pivot bush (5)',#25821,
#25630);
#25702=PRODUCT_DEFINITION('Pivot axle 160 mm','Pivot axle 160 mm',#25822,
#25630);
#25703=PRODUCT_DEFINITION('Axle end keeper (8)','Axle end keeper (8)',#25823,
#25630);
#25704=PRODUCT_DEFINITION('Axle end keeper (9)','Axle end keeper (9)',#25824,
#25630);
#25705=PRODUCT_DEFINITION('Axle distance sleeve 5 mm (9)',
'Axle distance sleeve 5 mm (9)',#25825,#25630);
#25706=PRODUCT_DEFINITION('Axle distance sleeve 5 mm (10)',
'Axle distance sleeve 5 mm (10)',#25826,#25630);
#25707=PRODUCT_DEFINITION('Axle distance sleeve 95 mm',
'Axle distance sleeve 95 mm',#25827,#25630);
#25708=PRODUCT_DEFINITION('Axle distance sleeve 10 mm (2)',
'Axle distance sleeve 10 mm (2)',#25828,#25630);
#25709=PRODUCT_DEFINITION('Axle distance sleeve 5 mm (11)',
'Axle distance sleeve 5 mm (11)',#25829,#25630);
#25710=PRODUCT_DEFINITION('Cap Screw - M4x16','Cap Screw - M4x16',#25830,
#25630);
#25711=PRODUCT_DEFINITION('Crossing arms','Crossing arms',#25831,#25630);
#25712=PRODUCT_DEFINITION('Crossing arm','Crossing arm',#25832,#25630);
#25713=PRODUCT_DEFINITION('Plain pivot bush (6)','Plain pivot bush (6)',#25833,
#25630);
#25714=PRODUCT_DEFINITION('Plain pivot bush (7)','Plain pivot bush (7)',#25834,
#25630);
#25715=PRODUCT_DEFINITION('Centre bearing retainer',
'Centre bearing retainer',#25835,#25630);
#25716=PRODUCT_DEFINITION('M4 low-profile retaining screw',
'M4 low-profile retaining screw',#25836,#25630);
#25717=PRODUCT_DEFINITION('M4 low-profile retaining screw (1)',
'M4 low-profile retaining screw (1)',#25837,#25630);
#25718=PRODUCT_DEFINITION('M4 low-profile retaining screw (2)',
'M4 low-profile retaining screw (2)',#25838,#25630);
#25719=PRODUCT_DEFINITION('M4 low-profile retaining screw (3)',
'M4 low-profile retaining screw (3)',#25839,#25630);
#25720=PRODUCT_DEFINITION('Centre bearing retainer (1)',
'Centre bearing retainer (1)',#25840,#25630);
#25721=PRODUCT_DEFINITION('M4 low-profile retaining screw (4)',
'M4 low-profile retaining screw (4)',#25841,#25630);
#25722=PRODUCT_DEFINITION('M4 low-profile retaining screw (5)',
'M4 low-profile retaining screw (5)',#25842,#25630);
#25723=PRODUCT_DEFINITION('M4 low-profile retaining screw (6)',
'M4 low-profile retaining screw (6)',#25843,#25630);
#25724=PRODUCT_DEFINITION('M4 low-profile retaining screw (7)',
'M4 low-profile retaining screw (7)',#25844,#25630);
#25725=PRODUCT_DEFINITION('Crossing arm (1)','Crossing arm (1)',#25845,#25630);
#25726=PRODUCT_DEFINITION('Plain pivot bush (8)','Plain pivot bush (8)',#25846,
#25630);
#25727=PRODUCT_DEFINITION('Plain pivot bush (9)','Plain pivot bush (9)',#25847,
#25630);
#25728=PRODUCT_DEFINITION('Centre bearing retainer (2)',
'Centre bearing retainer (2)',#25848,#25630);
#25729=PRODUCT_DEFINITION('M4 low-profile retaining screw (8)',
'M4 low-profile retaining screw (8)',#25849,#25630);
#25730=PRODUCT_DEFINITION('M4 low-profile retaining screw (9)',
'M4 low-profile retaining screw (9)',#25850,#25630);
#25731=PRODUCT_DEFINITION('M4 low-profile retaining screw (10)',
'M4 low-profile retaining screw (10)',#25851,#25630);
#25732=PRODUCT_DEFINITION('M4 low-profile retaining screw (11)',
'M4 low-profile retaining screw (11)',#25852,#25630);
#25733=PRODUCT_DEFINITION('Centre bearing retainer (3)',
'Centre bearing retainer (3)',#25853,#25630);
#25734=PRODUCT_DEFINITION('M4 low-profile retaining screw (12)',
'M4 low-profile retaining screw (12)',#25854,#25630);
#25735=PRODUCT_DEFINITION('M4 low-profile retaining screw (13)',
'M4 low-profile retaining screw (13)',#25855,#25630);
#25736=PRODUCT_DEFINITION('M4 low-profile retaining screw (14)',
'M4 low-profile retaining screw (14)',#25856,#25630);
#25737=PRODUCT_DEFINITION('M4 low-profile retaining screw (15)',
'M4 low-profile retaining screw (15)',#25857,#25630);
#25738=PRODUCT_DEFINITION('Sealed Ball Bearing - 12 x 32 x 10 mm',
'Sealed Ball Bearing - 12 x 32 x 10 mm',#25858,#25630);
#25739=PRODUCT_DEFINITION('Inner ring','Inner ring',#25859,#25630);
#25740=PRODUCT_DEFINITION('Outer ring','Outer ring',#25860,#25630);
#25741=PRODUCT_DEFINITION('Balls','Balls',#25861,#25630);
#25742=PRODUCT_DEFINITION('Cage','Cage',#25862,#25630);
#25743=PRODUCT_DEFINITION('Seals 2RS','Seals 2RS',#25863,#25630);
#25744=PRODUCT_DEFINITION('Lead screw and handwheel',
'Lead screw and handwheel',#25864,#25630);
#25745=PRODUCT_DEFINITION('Lead screw','Lead screw',#25865,#25630);
#25746=PRODUCT_DEFINITION('Bearing inner spacer','Bearing inner spacer',
#25866,#25630);
#25747=PRODUCT_DEFINITION('Bearing inner spacer (1)',
'Bearing inner spacer (1)',#25867,#25630);
#25748=PRODUCT_DEFINITION('Screw retaining collar',
'Screw retaining collar',#25868,#25630);
#25749=PRODUCT_DEFINITION('Screw retaining collar (1)',
'Screw retaining collar (1)',#25869,#25630);
#25750=PRODUCT_DEFINITION('Handwheel','Handwheel',#25870,#25630);
#25751=PRODUCT_DEFINITION_FORMATION('',$,#25994);
#25752=PRODUCT_DEFINITION_FORMATION('',$,#25995);
#25753=PRODUCT_DEFINITION_FORMATION('',$,#25996);
#25754=PRODUCT_DEFINITION_FORMATION('',$,#25997);
#25755=PRODUCT_DEFINITION_FORMATION('',$,#25998);
#25756=PRODUCT_DEFINITION_FORMATION('',$,#25999);
#25757=PRODUCT_DEFINITION_FORMATION('',$,#26000);
#25758=PRODUCT_DEFINITION_FORMATION('',$,#26001);
#25759=PRODUCT_DEFINITION_FORMATION('',$,#26002);
#25760=PRODUCT_DEFINITION_FORMATION('',$,#26003);
#25761=PRODUCT_DEFINITION_FORMATION('',$,#26004);
#25762=PRODUCT_DEFINITION_FORMATION('',$,#26005);
#25763=PRODUCT_DEFINITION_FORMATION('',$,#26006);
#25764=PRODUCT_DEFINITION_FORMATION('',$,#26007);
#25765=PRODUCT_DEFINITION_FORMATION('',$,#26008);
#25766=PRODUCT_DEFINITION_FORMATION('',$,#26009);
#25767=PRODUCT_DEFINITION_FORMATION('',$,#26010);
#25768=PRODUCT_DEFINITION_FORMATION('',$,#26011);
#25769=PRODUCT_DEFINITION_FORMATION('',$,#26012);
#25770=PRODUCT_DEFINITION_FORMATION('',$,#26013);
#25771=PRODUCT_DEFINITION_FORMATION('',$,#26014);
#25772=PRODUCT_DEFINITION_FORMATION('',$,#26015);
#25773=PRODUCT_DEFINITION_FORMATION('',$,#26016);
#25774=PRODUCT_DEFINITION_FORMATION('',$,#26017);
#25775=PRODUCT_DEFINITION_FORMATION('',$,#26018);
#25776=PRODUCT_DEFINITION_FORMATION('',$,#26019);
#25777=PRODUCT_DEFINITION_FORMATION('',$,#26020);
#25778=PRODUCT_DEFINITION_FORMATION('',$,#26021);
#25779=PRODUCT_DEFINITION_FORMATION('',$,#26022);
#25780=PRODUCT_DEFINITION_FORMATION('',$,#26023);
#25781=PRODUCT_DEFINITION_FORMATION('',$,#26024);
#25782=PRODUCT_DEFINITION_FORMATION('',$,#26025);
#25783=PRODUCT_DEFINITION_FORMATION('',$,#26026);
#25784=PRODUCT_DEFINITION_FORMATION('',$,#26027);
#25785=PRODUCT_DEFINITION_FORMATION('',$,#26028);
#25786=PRODUCT_DEFINITION_FORMATION('',$,#26029);
#25787=PRODUCT_DEFINITION_FORMATION('',$,#26030);
#25788=PRODUCT_DEFINITION_FORMATION('',$,#26031);
#25789=PRODUCT_DEFINITION_FORMATION('',$,#26032);
#25790=PRODUCT_DEFINITION_FORMATION('',$,#26033);
#25791=PRODUCT_DEFINITION_FORMATION('',$,#26034);
#25792=PRODUCT_DEFINITION_FORMATION('',$,#26035);
#25793=PRODUCT_DEFINITION_FORMATION('',$,#26036);
#25794=PRODUCT_DEFINITION_FORMATION('',$,#26037);
#25795=PRODUCT_DEFINITION_FORMATION('',$,#26038);
#25796=PRODUCT_DEFINITION_FORMATION('',$,#26039);
#25797=PRODUCT_DEFINITION_FORMATION('',$,#26040);
#25798=PRODUCT_DEFINITION_FORMATION('',$,#26041);
#25799=PRODUCT_DEFINITION_FORMATION('',$,#26042);
#25800=PRODUCT_DEFINITION_FORMATION('',$,#26043);
#25801=PRODUCT_DEFINITION_FORMATION('',$,#26044);
#25802=PRODUCT_DEFINITION_FORMATION('',$,#26045);
#25803=PRODUCT_DEFINITION_FORMATION('',$,#26046);
#25804=PRODUCT_DEFINITION_FORMATION('',$,#26047);
#25805=PRODUCT_DEFINITION_FORMATION('',$,#26048);
#25806=PRODUCT_DEFINITION_FORMATION('',$,#26049);
#25807=PRODUCT_DEFINITION_FORMATION('',$,#26050);
#25808=PRODUCT_DEFINITION_FORMATION('',$,#26051);
#25809=PRODUCT_DEFINITION_FORMATION('',$,#26052);
#25810=PRODUCT_DEFINITION_FORMATION('',$,#26053);
#25811=PRODUCT_DEFINITION_FORMATION('',$,#26054);
#25812=PRODUCT_DEFINITION_FORMATION('',$,#26055);
#25813=PRODUCT_DEFINITION_FORMATION('',$,#26056);
#25814=PRODUCT_DEFINITION_FORMATION('',$,#26057);
#25815=PRODUCT_DEFINITION_FORMATION('',$,#26058);
#25816=PRODUCT_DEFINITION_FORMATION('',$,#26059);
#25817=PRODUCT_DEFINITION_FORMATION('',$,#26060);
#25818=PRODUCT_DEFINITION_FORMATION('',$,#26061);
#25819=PRODUCT_DEFINITION_FORMATION('',$,#26062);
#25820=PRODUCT_DEFINITION_FORMATION('',$,#26063);
#25821=PRODUCT_DEFINITION_FORMATION('',$,#26064);
#25822=PRODUCT_DEFINITION_FORMATION('',$,#26065);
#25823=PRODUCT_DEFINITION_FORMATION('',$,#26066);
#25824=PRODUCT_DEFINITION_FORMATION('',$,#26067);
#25825=PRODUCT_DEFINITION_FORMATION('',$,#26068);
#25826=PRODUCT_DEFINITION_FORMATION('',$,#26069);
#25827=PRODUCT_DEFINITION_FORMATION('',$,#26070);
#25828=PRODUCT_DEFINITION_FORMATION('',$,#26071);
#25829=PRODUCT_DEFINITION_FORMATION('',$,#26072);
#25830=PRODUCT_DEFINITION_FORMATION('',$,#26073);
#25831=PRODUCT_DEFINITION_FORMATION('',$,#26074);
#25832=PRODUCT_DEFINITION_FORMATION('',$,#26075);
#25833=PRODUCT_DEFINITION_FORMATION('',$,#26076);
#25834=PRODUCT_DEFINITION_FORMATION('',$,#26077);
#25835=PRODUCT_DEFINITION_FORMATION('',$,#26078);
#25836=PRODUCT_DEFINITION_FORMATION('',$,#26079);
#25837=PRODUCT_DEFINITION_FORMATION('',$,#26080);
#25838=PRODUCT_DEFINITION_FORMATION('',$,#26081);
#25839=PRODUCT_DEFINITION_FORMATION('',$,#26082);
#25840=PRODUCT_DEFINITION_FORMATION('',$,#26083);
#25841=PRODUCT_DEFINITION_FORMATION('',$,#26084);
#25842=PRODUCT_DEFINITION_FORMATION('',$,#26085);
#25843=PRODUCT_DEFINITION_FORMATION('',$,#26086);
#25844=PRODUCT_DEFINITION_FORMATION('',$,#26087);
#25845=PRODUCT_DEFINITION_FORMATION('',$,#26088);
#25846=PRODUCT_DEFINITION_FORMATION('',$,#26089);
#25847=PRODUCT_DEFINITION_FORMATION('',$,#26090);
#25848=PRODUCT_DEFINITION_FORMATION('',$,#26091);
#25849=PRODUCT_DEFINITION_FORMATION('',$,#26092);
#25850=PRODUCT_DEFINITION_FORMATION('',$,#26093);
#25851=PRODUCT_DEFINITION_FORMATION('',$,#26094);
#25852=PRODUCT_DEFINITION_FORMATION('',$,#26095);
#25853=PRODUCT_DEFINITION_FORMATION('',$,#26096);
#25854=PRODUCT_DEFINITION_FORMATION('',$,#26097);
#25855=PRODUCT_DEFINITION_FORMATION('',$,#26098);
#25856=PRODUCT_DEFINITION_FORMATION('',$,#26099);
#25857=PRODUCT_DEFINITION_FORMATION('',$,#26100);
#25858=PRODUCT_DEFINITION_FORMATION('',$,#26101);
#25859=PRODUCT_DEFINITION_FORMATION('',$,#26102);
#25860=PRODUCT_DEFINITION_FORMATION('',$,#26103);
#25861=PRODUCT_DEFINITION_FORMATION('',$,#26104);
#25862=PRODUCT_DEFINITION_FORMATION('',$,#26105);
#25863=PRODUCT_DEFINITION_FORMATION('',$,#26106);
#25864=PRODUCT_DEFINITION_FORMATION('',$,#26107);
#25865=PRODUCT_DEFINITION_FORMATION('',$,#26108);
#25866=PRODUCT_DEFINITION_FORMATION('',$,#26109);
#25867=PRODUCT_DEFINITION_FORMATION('',$,#26110);
#25868=PRODUCT_DEFINITION_FORMATION('',$,#26111);
#25869=PRODUCT_DEFINITION_FORMATION('',$,#26112);
#25870=PRODUCT_DEFINITION_FORMATION('',$,#26113);
#25871=PRODUCT_RELATED_PRODUCT_CATEGORY(
'PAT-091','PAT-091',
(#25994));
#25872=PRODUCT_RELATED_PRODUCT_CATEGORY('Base and lower guides',
'Base and lower guides',(#25995));
#25873=PRODUCT_RELATED_PRODUCT_CATEGORY('Base plate','Base plate',(#25996));
#25874=PRODUCT_RELATED_PRODUCT_CATEGORY('Base foot','Base foot',(#25997));
#25875=PRODUCT_RELATED_PRODUCT_CATEGORY('Base foot (1)','Base foot (1)',
(#25998));
#25876=PRODUCT_RELATED_PRODUCT_CATEGORY('Lower pivot support',
'Lower pivot support',(#25999));
#25877=PRODUCT_RELATED_PRODUCT_CATEGORY('Screw bearing cap',
'Screw bearing cap',(#26000));
#25878=PRODUCT_RELATED_PRODUCT_CATEGORY('Screw bearing cap (1)',
'Screw bearing cap (1)',(#26001));
#25879=PRODUCT_RELATED_PRODUCT_CATEGORY('Lower screw support',
'Lower screw support',(#26002));
#25880=PRODUCT_RELATED_PRODUCT_CATEGORY('Screw bearing cap (2)',
'Screw bearing cap (2)',(#26003));
#25881=PRODUCT_RELATED_PRODUCT_CATEGORY('Screw bearing cap (3)',
'Screw bearing cap (3)',(#26004));
#25882=PRODUCT_RELATED_PRODUCT_CATEGORY('Guide shaft','Guide shaft',(#26005));
#25883=PRODUCT_RELATED_PRODUCT_CATEGORY('Guide shaft (1)',
'Guide shaft (1)',(#26006));
#25884=PRODUCT_RELATED_PRODUCT_CATEGORY('Pivot axle 140 mm',
'Pivot axle 140 mm',(#26007));
#25885=PRODUCT_RELATED_PRODUCT_CATEGORY('Axle end keeper',
'Axle end keeper',(#26008));
#25886=PRODUCT_RELATED_PRODUCT_CATEGORY('Axle end keeper (1)',
'Axle end keeper (1)',(#26009));
#25887=PRODUCT_RELATED_PRODUCT_CATEGORY('Axle distance sleeve 5 mm',
'Axle distance sleeve 5 mm',(#26010));
#25888=PRODUCT_RELATED_PRODUCT_CATEGORY('Axle distance sleeve 10 mm',
'Axle distance sleeve 10 mm',(#26011));
#25889=PRODUCT_RELATED_PRODUCT_CATEGORY('Axle distance sleeve 5 mm (1)',
'Axle distance sleeve 5 mm (1)',(#26012));
#25890=PRODUCT_RELATED_PRODUCT_CATEGORY('M4x10 Cap Screw',
'M4x10 Cap Screw',(#26013));
#25891=PRODUCT_RELATED_PRODUCT_CATEGORY('Top and upper guides',
'Top and upper guides',(#26014));
#25892=PRODUCT_RELATED_PRODUCT_CATEGORY('Top plate','Top plate',(#26015));
#25893=PRODUCT_RELATED_PRODUCT_CATEGORY('Upper fixed end support',
'Upper fixed end support',(#26016));
#25894=PRODUCT_RELATED_PRODUCT_CATEGORY('Upper sliding end support',
'Upper sliding end support',(#26017));
#25895=PRODUCT_RELATED_PRODUCT_CATEGORY('Guide shaft (2)',
'Guide shaft (2)',(#26018));
#25896=PRODUCT_RELATED_PRODUCT_CATEGORY('Guide shaft (3)',
'Guide shaft (3)',(#26019));
#25897=PRODUCT_RELATED_PRODUCT_CATEGORY('Pivot axle 145 mm',
'Pivot axle 145 mm',(#26020));
#25898=PRODUCT_RELATED_PRODUCT_CATEGORY('Axle end keeper (2)',
'Axle end keeper (2)',(#26021));
#25899=PRODUCT_RELATED_PRODUCT_CATEGORY('Axle end keeper (3)',
'Axle end keeper (3)',(#26022));
#25900=PRODUCT_RELATED_PRODUCT_CATEGORY('Axle distance sleeve 5 mm (2)',
'Axle distance sleeve 5 mm (2)',(#26023));
#25901=PRODUCT_RELATED_PRODUCT_CATEGORY('Axle distance sleeve 5 mm (3)',
'Axle distance sleeve 5 mm (3)',(#26024));
#25902=PRODUCT_RELATED_PRODUCT_CATEGORY('Axle distance sleeve 30 mm',
'Axle distance sleeve 30 mm',(#26025));
#25903=PRODUCT_RELATED_PRODUCT_CATEGORY('Axle distance sleeve 5 mm (4)',
'Axle distance sleeve 5 mm (4)',(#26026));
#25904=PRODUCT_RELATED_PRODUCT_CATEGORY('Cap Screw - M5x20',
'Cap Screw - M5x20',(#26027));
#25905=PRODUCT_RELATED_PRODUCT_CATEGORY('Lower sliding pivot',
'Lower sliding pivot',(#26028));
#25906=PRODUCT_RELATED_PRODUCT_CATEGORY('Lower nut carriage',
'Lower nut carriage',(#26029));
#25907=PRODUCT_RELATED_PRODUCT_CATEGORY('Linear bearing keeper',
'Linear bearing keeper',(#26030));
#25908=PRODUCT_RELATED_PRODUCT_CATEGORY('Linear bearing keeper (1)',
'Linear bearing keeper (1)',(#26031));
#25909=PRODUCT_RELATED_PRODUCT_CATEGORY('Sliding pivot crosshead',
'Sliding pivot crosshead',(#26032));
#25910=PRODUCT_RELATED_PRODUCT_CATEGORY('Pivot axle 145 mm (1)',
'Pivot axle 145 mm (1)',(#26033));
#25911=PRODUCT_RELATED_PRODUCT_CATEGORY('Axle end keeper (4)',
'Axle end keeper (4)',(#26034));
#25912=PRODUCT_RELATED_PRODUCT_CATEGORY('Axle end keeper (5)',
'Axle end keeper (5)',(#26035));
#25913=PRODUCT_RELATED_PRODUCT_CATEGORY('Axle distance sleeve 5 mm (5)',
'Axle distance sleeve 5 mm (5)',(#26036));
#25914=PRODUCT_RELATED_PRODUCT_CATEGORY(
'Axle distance sleeve 10 mm (1)','Axle distance sleeve 10 mm (1)',(#26037));
#25915=PRODUCT_RELATED_PRODUCT_CATEGORY('Axle distance sleeve 35 mm',
'Axle distance sleeve 35 mm',(#26038));
#25916=PRODUCT_RELATED_PRODUCT_CATEGORY('Axle distance sleeve 5 mm (6)',
'Axle distance sleeve 5 mm (6)',(#26039));
#25917=PRODUCT_RELATED_PRODUCT_CATEGORY('Upper sliding pivot',
'Upper sliding pivot',(#26040));
#25918=PRODUCT_RELATED_PRODUCT_CATEGORY('Upper sliding carriage',
'Upper sliding carriage',(#26041));
#25919=PRODUCT_RELATED_PRODUCT_CATEGORY('Linear bearing keeper (2)',
'Linear bearing keeper (2)',(#26042));
#25920=PRODUCT_RELATED_PRODUCT_CATEGORY('Linear bearing keeper (3)',
'Linear bearing keeper (3)',(#26043));
#25921=PRODUCT_RELATED_PRODUCT_CATEGORY('Sliding pivot crosshead (1)',
'Sliding pivot crosshead (1)',(#26044));
#25922=PRODUCT_RELATED_PRODUCT_CATEGORY('Pivot axle 140 mm (1)',
'Pivot axle 140 mm (1)',(#26045));
#25923=PRODUCT_RELATED_PRODUCT_CATEGORY('Axle end keeper (6)',
'Axle end keeper (6)',(#26046));
#25924=PRODUCT_RELATED_PRODUCT_CATEGORY('Axle end keeper (7)',
'Axle end keeper (7)',(#26047));
#25925=PRODUCT_RELATED_PRODUCT_CATEGORY('Axle distance sleeve 5 mm (7)',
'Axle distance sleeve 5 mm (7)',(#26048));
#25926=PRODUCT_RELATED_PRODUCT_CATEGORY('Axle distance sleeve 25 mm',
'Axle distance sleeve 25 mm',(#26049));
#25927=PRODUCT_RELATED_PRODUCT_CATEGORY('Axle distance sleeve 15 mm',
'Axle distance sleeve 15 mm',(#26050));
#25928=PRODUCT_RELATED_PRODUCT_CATEGORY('Axle distance sleeve 5 mm (8)',
'Axle distance sleeve 5 mm (8)',(#26051));
#25929=PRODUCT_RELATED_PRODUCT_CATEGORY(
'Linear Ball Bushing - 12 x 21 x 30 mm',
'Linear Ball Bushing - 12 x 21 x 30 mm',(#26052));
#25930=PRODUCT_RELATED_PRODUCT_CATEGORY('Steel sleeve','Steel sleeve',(#26053));
#25931=PRODUCT_RELATED_PRODUCT_CATEGORY('Ball retainer (plastic)',
'Ball retainer (plastic)',(#26054));
#25932=PRODUCT_RELATED_PRODUCT_CATEGORY('M4x4 collar screw',
'M4x4 collar screw',(#26055));
#25933=PRODUCT_RELATED_PRODUCT_CATEGORY('Rising arms','Rising arms',(#26056));
#25934=PRODUCT_RELATED_PRODUCT_CATEGORY('Rising arm','Rising arm',(#26057));
#25935=PRODUCT_RELATED_PRODUCT_CATEGORY('Plain pivot bush',
'Plain pivot bush',(#26058));
#25936=PRODUCT_RELATED_PRODUCT_CATEGORY('Plain pivot bush (1)',
'Plain pivot bush (1)',(#26059));
#25937=PRODUCT_RELATED_PRODUCT_CATEGORY('Plain pivot bush (2)',
'Plain pivot bush (2)',(#26060));
#25938=PRODUCT_RELATED_PRODUCT_CATEGORY('Rising arm (1)',
'Rising arm (1)',(#26061));
#25939=PRODUCT_RELATED_PRODUCT_CATEGORY('Plain pivot bush (3)',
'Plain pivot bush (3)',(#26062));
#25940=PRODUCT_RELATED_PRODUCT_CATEGORY('Plain pivot bush (4)',
'Plain pivot bush (4)',(#26063));
#25941=PRODUCT_RELATED_PRODUCT_CATEGORY('Plain pivot bush (5)',
'Plain pivot bush (5)',(#26064));
#25942=PRODUCT_RELATED_PRODUCT_CATEGORY('Pivot axle 160 mm',
'Pivot axle 160 mm',(#26065));
#25943=PRODUCT_RELATED_PRODUCT_CATEGORY('Axle end keeper (8)',
'Axle end keeper (8)',(#26066));
#25944=PRODUCT_RELATED_PRODUCT_CATEGORY('Axle end keeper (9)',
'Axle end keeper (9)',(#26067));
#25945=PRODUCT_RELATED_PRODUCT_CATEGORY('Axle distance sleeve 5 mm (9)',
'Axle distance sleeve 5 mm (9)',(#26068));
#25946=PRODUCT_RELATED_PRODUCT_CATEGORY(
'Axle distance sleeve 5 mm (10)','Axle distance sleeve 5 mm (10)',(#26069));
#25947=PRODUCT_RELATED_PRODUCT_CATEGORY('Axle distance sleeve 95 mm',
'Axle distance sleeve 95 mm',(#26070));
#25948=PRODUCT_RELATED_PRODUCT_CATEGORY(
'Axle distance sleeve 10 mm (2)','Axle distance sleeve 10 mm (2)',(#26071));
#25949=PRODUCT_RELATED_PRODUCT_CATEGORY(
'Axle distance sleeve 5 mm (11)','Axle distance sleeve 5 mm (11)',(#26072));
#25950=PRODUCT_RELATED_PRODUCT_CATEGORY('Cap Screw - M4x16',
'Cap Screw - M4x16',(#26073));
#25951=PRODUCT_RELATED_PRODUCT_CATEGORY('Crossing arms','Crossing arms',
(#26074));
#25952=PRODUCT_RELATED_PRODUCT_CATEGORY('Crossing arm','Crossing arm',(#26075));
#25953=PRODUCT_RELATED_PRODUCT_CATEGORY('Plain pivot bush (6)',
'Plain pivot bush (6)',(#26076));
#25954=PRODUCT_RELATED_PRODUCT_CATEGORY('Plain pivot bush (7)',
'Plain pivot bush (7)',(#26077));
#25955=PRODUCT_RELATED_PRODUCT_CATEGORY('Centre bearing retainer',
'Centre bearing retainer',(#26078));
#25956=PRODUCT_RELATED_PRODUCT_CATEGORY(
'M4 low-profile retaining screw','M4 low-profile retaining screw',(#26079));
#25957=PRODUCT_RELATED_PRODUCT_CATEGORY(
'M4 low-profile retaining screw (1)',
'M4 low-profile retaining screw (1)',(#26080));
#25958=PRODUCT_RELATED_PRODUCT_CATEGORY(
'M4 low-profile retaining screw (2)',
'M4 low-profile retaining screw (2)',(#26081));
#25959=PRODUCT_RELATED_PRODUCT_CATEGORY(
'M4 low-profile retaining screw (3)',
'M4 low-profile retaining screw (3)',(#26082));
#25960=PRODUCT_RELATED_PRODUCT_CATEGORY('Centre bearing retainer (1)',
'Centre bearing retainer (1)',(#26083));
#25961=PRODUCT_RELATED_PRODUCT_CATEGORY(
'M4 low-profile retaining screw (4)',
'M4 low-profile retaining screw (4)',(#26084));
#25962=PRODUCT_RELATED_PRODUCT_CATEGORY(
'M4 low-profile retaining screw (5)',
'M4 low-profile retaining screw (5)',(#26085));
#25963=PRODUCT_RELATED_PRODUCT_CATEGORY(
'M4 low-profile retaining screw (6)',
'M4 low-profile retaining screw (6)',(#26086));
#25964=PRODUCT_RELATED_PRODUCT_CATEGORY(
'M4 low-profile retaining screw (7)',
'M4 low-profile retaining screw (7)',(#26087));
#25965=PRODUCT_RELATED_PRODUCT_CATEGORY('Crossing arm (1)',
'Crossing arm (1)',(#26088));
#25966=PRODUCT_RELATED_PRODUCT_CATEGORY('Plain pivot bush (8)',
'Plain pivot bush (8)',(#26089));
#25967=PRODUCT_RELATED_PRODUCT_CATEGORY('Plain pivot bush (9)',
'Plain pivot bush (9)',(#26090));
#25968=PRODUCT_RELATED_PRODUCT_CATEGORY('Centre bearing retainer (2)',
'Centre bearing retainer (2)',(#26091));
#25969=PRODUCT_RELATED_PRODUCT_CATEGORY(
'M4 low-profile retaining screw (8)',
'M4 low-profile retaining screw (8)',(#26092));
#25970=PRODUCT_RELATED_PRODUCT_CATEGORY(
'M4 low-profile retaining screw (9)',
'M4 low-profile retaining screw (9)',(#26093));
#25971=PRODUCT_RELATED_PRODUCT_CATEGORY(
'M4 low-profile retaining screw (10)',
'M4 low-profile retaining screw (10)',(#26094));
#25972=PRODUCT_RELATED_PRODUCT_CATEGORY(
'M4 low-profile retaining screw (11)',
'M4 low-profile retaining screw (11)',(#26095));
#25973=PRODUCT_RELATED_PRODUCT_CATEGORY('Centre bearing retainer (3)',
'Centre bearing retainer (3)',(#26096));
#25974=PRODUCT_RELATED_PRODUCT_CATEGORY(
'M4 low-profile retaining screw (12)',
'M4 low-profile retaining screw (12)',(#26097));
#25975=PRODUCT_RELATED_PRODUCT_CATEGORY(
'M4 low-profile retaining screw (13)',
'M4 low-profile retaining screw (13)',(#26098));
#25976=PRODUCT_RELATED_PRODUCT_CATEGORY(
'M4 low-profile retaining screw (14)',
'M4 low-profile retaining screw (14)',(#26099));
#25977=PRODUCT_RELATED_PRODUCT_CATEGORY(
'M4 low-profile retaining screw (15)',
'M4 low-profile retaining screw (15)',(#26100));
#25978=PRODUCT_RELATED_PRODUCT_CATEGORY(
'Sealed Ball Bearing - 12 x 32 x 10 mm',
'Sealed Ball Bearing - 12 x 32 x 10 mm',(#26101));
#25979=PRODUCT_RELATED_PRODUCT_CATEGORY('Inner ring','Inner ring',(#26102));
#25980=PRODUCT_RELATED_PRODUCT_CATEGORY('Outer ring','Outer ring',(#26103));
#25981=PRODUCT_RELATED_PRODUCT_CATEGORY('Balls','Balls',(#26104));
#25982=PRODUCT_RELATED_PRODUCT_CATEGORY('Cage','Cage',(#26105));
#25983=PRODUCT_RELATED_PRODUCT_CATEGORY('Seals 2RS','Seals 2RS',(#26106));
#25984=PRODUCT_RELATED_PRODUCT_CATEGORY('Lead screw and handwheel',
'Lead screw and handwheel',(#26107));
#25985=PRODUCT_RELATED_PRODUCT_CATEGORY('Lead screw','Lead screw',(#26108));
#25986=PRODUCT_RELATED_PRODUCT_CATEGORY('Bearing inner spacer',
'Bearing inner spacer',(#26109));
#25987=PRODUCT_RELATED_PRODUCT_CATEGORY('Bearing inner spacer (1)',
'Bearing inner spacer (1)',(#26110));
#25988=PRODUCT_RELATED_PRODUCT_CATEGORY('Screw retaining collar',
'Screw retaining collar',(#26111));
#25989=PRODUCT_RELATED_PRODUCT_CATEGORY('Screw retaining collar (1)',
'Screw retaining collar (1)',(#26112));
#25990=PRODUCT_RELATED_PRODUCT_CATEGORY('Handwheel','Handwheel',(#26113));
#25991=APPLICATION_PROTOCOL_DEFINITION('international standard',
'automotive_design',2009,#25992);
#25992=APPLICATION_CONTEXT(
'Core Data for Automotive Mechanical Design Process');
#25993=PRODUCT_CONTEXT('part definition',#25992,'mechanical');
#25994=PRODUCT('PAT-091',
'PAT-091','PAT-091',
(#25993));
#25995=PRODUCT('Base and lower guides','Base and lower guides',
'Base and lower guides',(#25993));
#25996=PRODUCT('Base plate','Base plate','Base plate',(#25993));
#25997=PRODUCT('Base foot','Base foot','Base foot',(#25993));
#25998=PRODUCT('Base foot (1)','Base foot (1)','Base foot (1)',(#25993));
#25999=PRODUCT('Lower pivot support','Lower pivot support',
'Lower pivot support',(#25993));
#26000=PRODUCT('Screw bearing cap','Screw bearing cap',
'Screw bearing cap',(#25993));
#26001=PRODUCT('Screw bearing cap (1)','Screw bearing cap (1)',
'Screw bearing cap (1)',(#25993));
#26002=PRODUCT('Lower screw support','Lower screw support',
'Lower screw support',(#25993));
#26003=PRODUCT('Screw bearing cap (2)','Screw bearing cap (2)',
'Screw bearing cap (2)',(#25993));
#26004=PRODUCT('Screw bearing cap (3)','Screw bearing cap (3)',
'Screw bearing cap (3)',(#25993));
#26005=PRODUCT('Guide shaft','Guide shaft','Guide shaft',(#25993));
#26006=PRODUCT('Guide shaft (1)','Guide shaft (1)','Guide shaft (1)',(#25993));
#26007=PRODUCT('Pivot axle 140 mm','Pivot axle 140 mm',
'Pivot axle 140 mm',(#25993));
#26008=PRODUCT('Axle end keeper','Axle end keeper','Axle end keeper',(#25993));
#26009=PRODUCT('Axle end keeper (1)','Axle end keeper (1)',
'Axle end keeper (1)',(#25993));
#26010=PRODUCT('Axle distance sleeve 5 mm','Axle distance sleeve 5 mm',
'Axle distance sleeve 5 mm',(#25993));
#26011=PRODUCT('Axle distance sleeve 10 mm',
'Axle distance sleeve 10 mm','Axle distance sleeve 10 mm',(#25993));
#26012=PRODUCT('Axle distance sleeve 5 mm (1)',
'Axle distance sleeve 5 mm (1)','Axle distance sleeve 5 mm (1)',(#25993));
#26013=PRODUCT('M4x10 Cap Screw','M4x10 Cap Screw','M4x10 Cap Screw',(#25993));
#26014=PRODUCT('Top and upper guides','Top and upper guides',
'Top and upper guides',(#25993));
#26015=PRODUCT('Top plate','Top plate','Top plate',(#25993));
#26016=PRODUCT('Upper fixed end support','Upper fixed end support',
'Upper fixed end support',(#25993));
#26017=PRODUCT('Upper sliding end support','Upper sliding end support',
'Upper sliding end support',(#25993));
#26018=PRODUCT('Guide shaft (2)','Guide shaft (2)','Guide shaft (2)',(#25993));
#26019=PRODUCT('Guide shaft (3)','Guide shaft (3)','Guide shaft (3)',(#25993));
#26020=PRODUCT('Pivot axle 145 mm','Pivot axle 145 mm',
'Pivot axle 145 mm',(#25993));
#26021=PRODUCT('Axle end keeper (2)','Axle end keeper (2)',
'Axle end keeper (2)',(#25993));
#26022=PRODUCT('Axle end keeper (3)','Axle end keeper (3)',
'Axle end keeper (3)',(#25993));
#26023=PRODUCT('Axle distance sleeve 5 mm (2)',
'Axle distance sleeve 5 mm (2)','Axle distance sleeve 5 mm (2)',(#25993));
#26024=PRODUCT('Axle distance sleeve 5 mm (3)',
'Axle distance sleeve 5 mm (3)','Axle distance sleeve 5 mm (3)',(#25993));
#26025=PRODUCT('Axle distance sleeve 30 mm',
'Axle distance sleeve 30 mm','Axle distance sleeve 30 mm',(#25993));
#26026=PRODUCT('Axle distance sleeve 5 mm (4)',
'Axle distance sleeve 5 mm (4)','Axle distance sleeve 5 mm (4)',(#25993));
#26027=PRODUCT('Cap Screw - M5x20','Cap Screw - M5x20',
'Cap Screw - M5x20',(#25993));
#26028=PRODUCT('Lower sliding pivot','Lower sliding pivot',
'Lower sliding pivot',(#25993));
#26029=PRODUCT('Lower nut carriage','Lower nut carriage',
'Lower nut carriage',(#25993));
#26030=PRODUCT('Linear bearing keeper','Linear bearing keeper',
'Linear bearing keeper',(#25993));
#26031=PRODUCT('Linear bearing keeper (1)','Linear bearing keeper (1)',
'Linear bearing keeper (1)',(#25993));
#26032=PRODUCT('Sliding pivot crosshead','Sliding pivot crosshead',
'Sliding pivot crosshead',(#25993));
#26033=PRODUCT('Pivot axle 145 mm (1)','Pivot axle 145 mm (1)',
'Pivot axle 145 mm (1)',(#25993));
#26034=PRODUCT('Axle end keeper (4)','Axle end keeper (4)',
'Axle end keeper (4)',(#25993));
#26035=PRODUCT('Axle end keeper (5)','Axle end keeper (5)',
'Axle end keeper (5)',(#25993));
#26036=PRODUCT('Axle distance sleeve 5 mm (5)',
'Axle distance sleeve 5 mm (5)','Axle distance sleeve 5 mm (5)',(#25993));
#26037=PRODUCT('Axle distance sleeve 10 mm (1)',
'Axle distance sleeve 10 mm (1)','Axle distance sleeve 10 mm (1)',(#25993));
#26038=PRODUCT('Axle distance sleeve 35 mm',
'Axle distance sleeve 35 mm','Axle distance sleeve 35 mm',(#25993));
#26039=PRODUCT('Axle distance sleeve 5 mm (6)',
'Axle distance sleeve 5 mm (6)','Axle distance sleeve 5 mm (6)',(#25993));
#26040=PRODUCT('Upper sliding pivot','Upper sliding pivot',
'Upper sliding pivot',(#25993));
#26041=PRODUCT('Upper sliding carriage','Upper sliding carriage',
'Upper sliding carriage',(#25993));
#26042=PRODUCT('Linear bearing keeper (2)','Linear bearing keeper (2)',
'Linear bearing keeper (2)',(#25993));
#26043=PRODUCT('Linear bearing keeper (3)','Linear bearing keeper (3)',
'Linear bearing keeper (3)',(#25993));
#26044=PRODUCT('Sliding pivot crosshead (1)',
'Sliding pivot crosshead (1)','Sliding pivot crosshead (1)',(#25993));
#26045=PRODUCT('Pivot axle 140 mm (1)','Pivot axle 140 mm (1)',
'Pivot axle 140 mm (1)',(#25993));
#26046=PRODUCT('Axle end keeper (6)','Axle end keeper (6)',
'Axle end keeper (6)',(#25993));
#26047=PRODUCT('Axle end keeper (7)','Axle end keeper (7)',
'Axle end keeper (7)',(#25993));
#26048=PRODUCT('Axle distance sleeve 5 mm (7)',
'Axle distance sleeve 5 mm (7)','Axle distance sleeve 5 mm (7)',(#25993));
#26049=PRODUCT('Axle distance sleeve 25 mm',
'Axle distance sleeve 25 mm','Axle distance sleeve 25 mm',(#25993));
#26050=PRODUCT('Axle distance sleeve 15 mm',
'Axle distance sleeve 15 mm','Axle distance sleeve 15 mm',(#25993));
#26051=PRODUCT('Axle distance sleeve 5 mm (8)',
'Axle distance sleeve 5 mm (8)','Axle distance sleeve 5 mm (8)',(#25993));
#26052=PRODUCT('Linear Ball Bushing - 12 x 21 x 30 mm',
'Linear Ball Bushing - 12 x 21 x 30 mm',
'Linear Ball Bushing - 12 x 21 x 30 mm',(#25993));
#26053=PRODUCT('Steel sleeve','Steel sleeve','Steel sleeve',(#25993));
#26054=PRODUCT('Ball retainer (plastic)','Ball retainer (plastic)',
'Ball retainer (plastic)',(#25993));
#26055=PRODUCT('M4x4 collar screw','M4x4 collar screw',
'M4x4 collar screw',(#25993));
#26056=PRODUCT('Rising arms','Rising arms','Rising arms',(#25993));
#26057=PRODUCT('Rising arm','Rising arm','Rising arm',(#25993));
#26058=PRODUCT('Plain pivot bush','Plain pivot bush','Plain pivot bush',
(#25993));
#26059=PRODUCT('Plain pivot bush (1)','Plain pivot bush (1)',
'Plain pivot bush (1)',(#25993));
#26060=PRODUCT('Plain pivot bush (2)','Plain pivot bush (2)',
'Plain pivot bush (2)',(#25993));
#26061=PRODUCT('Rising arm (1)','Rising arm (1)','Rising arm (1)',(#25993));
#26062=PRODUCT('Plain pivot bush (3)','Plain pivot bush (3)',
'Plain pivot bush (3)',(#25993));
#26063=PRODUCT('Plain pivot bush (4)','Plain pivot bush (4)',
'Plain pivot bush (4)',(#25993));
#26064=PRODUCT('Plain pivot bush (5)','Plain pivot bush (5)',
'Plain pivot bush (5)',(#25993));
#26065=PRODUCT('Pivot axle 160 mm','Pivot axle 160 mm',
'Pivot axle 160 mm',(#25993));
#26066=PRODUCT('Axle end keeper (8)','Axle end keeper (8)',
'Axle end keeper (8)',(#25993));
#26067=PRODUCT('Axle end keeper (9)','Axle end keeper (9)',
'Axle end keeper (9)',(#25993));
#26068=PRODUCT('Axle distance sleeve 5 mm (9)',
'Axle distance sleeve 5 mm (9)','Axle distance sleeve 5 mm (9)',(#25993));
#26069=PRODUCT('Axle distance sleeve 5 mm (10)',
'Axle distance sleeve 5 mm (10)','Axle distance sleeve 5 mm (10)',(#25993));
#26070=PRODUCT('Axle distance sleeve 95 mm',
'Axle distance sleeve 95 mm','Axle distance sleeve 95 mm',(#25993));
#26071=PRODUCT('Axle distance sleeve 10 mm (2)',
'Axle distance sleeve 10 mm (2)','Axle distance sleeve 10 mm (2)',(#25993));
#26072=PRODUCT('Axle distance sleeve 5 mm (11)',
'Axle distance sleeve 5 mm (11)','Axle distance sleeve 5 mm (11)',(#25993));
#26073=PRODUCT('Cap Screw - M4x16','Cap Screw - M4x16',
'Cap Screw - M4x16',(#25993));
#26074=PRODUCT('Crossing arms','Crossing arms','Crossing arms',(#25993));
#26075=PRODUCT('Crossing arm','Crossing arm','Crossing arm',(#25993));
#26076=PRODUCT('Plain pivot bush (6)','Plain pivot bush (6)',
'Plain pivot bush (6)',(#25993));
#26077=PRODUCT('Plain pivot bush (7)','Plain pivot bush (7)',
'Plain pivot bush (7)',(#25993));
#26078=PRODUCT('Centre bearing retainer','Centre bearing retainer',
'Centre bearing retainer',(#25993));
#26079=PRODUCT('M4 low-profile retaining screw',
'M4 low-profile retaining screw','M4 low-profile retaining screw',(#25993));
#26080=PRODUCT('M4 low-profile retaining screw (1)',
'M4 low-profile retaining screw (1)','M4 low-profile retaining screw (1)',(#25993));
#26081=PRODUCT('M4 low-profile retaining screw (2)',
'M4 low-profile retaining screw (2)','M4 low-profile retaining screw (2)',(#25993));
#26082=PRODUCT('M4 low-profile retaining screw (3)',
'M4 low-profile retaining screw (3)','M4 low-profile retaining screw (3)',(#25993));
#26083=PRODUCT('Centre bearing retainer (1)',
'Centre bearing retainer (1)','Centre bearing retainer (1)',(#25993));
#26084=PRODUCT('M4 low-profile retaining screw (4)',
'M4 low-profile retaining screw (4)','M4 low-profile retaining screw (4)',(#25993));
#26085=PRODUCT('M4 low-profile retaining screw (5)',
'M4 low-profile retaining screw (5)','M4 low-profile retaining screw (5)',(#25993));
#26086=PRODUCT('M4 low-profile retaining screw (6)',
'M4 low-profile retaining screw (6)','M4 low-profile retaining screw (6)',(#25993));
#26087=PRODUCT('M4 low-profile retaining screw (7)',
'M4 low-profile retaining screw (7)','M4 low-profile retaining screw (7)',(#25993));
#26088=PRODUCT('Crossing arm (1)','Crossing arm (1)','Crossing arm (1)',(#25993));
#26089=PRODUCT('Plain pivot bush (8)','Plain pivot bush (8)',
'Plain pivot bush (8)',(#25993));
#26090=PRODUCT('Plain pivot bush (9)','Plain pivot bush (9)',
'Plain pivot bush (9)',(#25993));
#26091=PRODUCT('Centre bearing retainer (2)',
'Centre bearing retainer (2)','Centre bearing retainer (2)',(#25993));
#26092=PRODUCT('M4 low-profile retaining screw (8)',
'M4 low-profile retaining screw (8)','M4 low-profile retaining screw (8)',(#25993));
#26093=PRODUCT('M4 low-profile retaining screw (9)',
'M4 low-profile retaining screw (9)','M4 low-profile retaining screw (9)',(#25993));
#26094=PRODUCT('M4 low-profile retaining screw (10)',
'M4 low-profile retaining screw (10)','M4 low-profile retaining screw (10)',
(#25993));
#26095=PRODUCT('M4 low-profile retaining screw (11)',
'M4 low-profile retaining screw (11)','M4 low-profile retaining screw (11)',
(#25993));
#26096=PRODUCT('Centre bearing retainer (3)',
'Centre bearing retainer (3)','Centre bearing retainer (3)',(#25993));
#26097=PRODUCT('M4 low-profile retaining screw (12)',
'M4 low-profile retaining screw (12)','M4 low-profile retaining screw (12)',
(#25993));
#26098=PRODUCT('M4 low-profile retaining screw (13)',
'M4 low-profile retaining screw (13)','M4 low-profile retaining screw (13)',
(#25993));
#26099=PRODUCT('M4 low-profile retaining screw (14)',
'M4 low-profile retaining screw (14)','M4 low-profile retaining screw (14)',
(#25993));
#26100=PRODUCT('M4 low-profile retaining screw (15)',
'M4 low-profile retaining screw (15)','M4 low-profile retaining screw (15)',
(#25993));
#26101=PRODUCT('Sealed Ball Bearing - 12 x 32 x 10 mm',
'Sealed Ball Bearing - 12 x 32 x 10 mm',
'Sealed Ball Bearing - 12 x 32 x 10 mm',(#25993));
#26102=PRODUCT('Inner ring','Inner ring','Inner ring',(#25993));
#26103=PRODUCT('Outer ring','Outer ring','Outer ring',(#25993));
#26104=PRODUCT('Balls','Balls','Balls',(#25993));
#26105=PRODUCT('Cage','Cage','Cage',(#25993));
#26106=PRODUCT('Seals 2RS','Seals 2RS','Seals 2RS',(#25993));
#26107=PRODUCT('Lead screw and handwheel','Lead screw and handwheel',
'Lead screw and handwheel',(#25993));
#26108=PRODUCT('Lead screw','Lead screw','Lead screw',(#25993));
#26109=PRODUCT('Bearing inner spacer','Bearing inner spacer',
'Bearing inner spacer',(#25993));
#26110=PRODUCT('Bearing inner spacer (1)','Bearing inner spacer (1)',
'Bearing inner spacer (1)',(#25993));
#26111=PRODUCT('Screw retaining collar','Screw retaining collar',
'Screw retaining collar',(#25993));
#26112=PRODUCT('Screw retaining collar (1)','Screw retaining collar (1)',
'Screw retaining collar (1)',(#25993));
#26113=PRODUCT('Handwheel','Handwheel','Handwheel',(#25993));
#26114=PRESENTATION_STYLE_ASSIGNMENT((#26122));
#26115=PRESENTATION_STYLE_ASSIGNMENT((#26123));
#26116=PRESENTATION_STYLE_ASSIGNMENT((#26124));
#26117=PRESENTATION_STYLE_ASSIGNMENT((#26125));
#26118=PRESENTATION_STYLE_ASSIGNMENT((#26126));
#26119=PRESENTATION_STYLE_ASSIGNMENT((#26127));
#26120=PRESENTATION_STYLE_ASSIGNMENT((#26128));
#26121=PRESENTATION_STYLE_ASSIGNMENT((NULL_STYLE(.NULL.)));
#26122=SURFACE_STYLE_USAGE(.BOTH.,#26129);
#26123=SURFACE_STYLE_USAGE(.BOTH.,#26130);
#26124=SURFACE_STYLE_USAGE(.BOTH.,#26131);
#26125=SURFACE_STYLE_USAGE(.BOTH.,#26132);
#26126=SURFACE_STYLE_USAGE(.BOTH.,#26133);
#26127=SURFACE_STYLE_USAGE(.BOTH.,#26134);
#26128=SURFACE_STYLE_USAGE(.BOTH.,#26135);
#26129=SURFACE_SIDE_STYLE('',(#26136));
#26130=SURFACE_SIDE_STYLE('',(#26137));
#26131=SURFACE_SIDE_STYLE('',(#26138));
#26132=SURFACE_SIDE_STYLE('',(#26139));
#26133=SURFACE_SIDE_STYLE('',(#26140));
#26134=SURFACE_SIDE_STYLE('',(#26141));
#26135=SURFACE_SIDE_STYLE('',(#26142));
#26136=SURFACE_STYLE_FILL_AREA(#26143);
#26137=SURFACE_STYLE_FILL_AREA(#26144);
#26138=SURFACE_STYLE_FILL_AREA(#26145);
#26139=SURFACE_STYLE_FILL_AREA(#26146);
#26140=SURFACE_STYLE_FILL_AREA(#26147);
#26141=SURFACE_STYLE_FILL_AREA(#26148);
#26142=SURFACE_STYLE_FILL_AREA(#26149);
#26143=FILL_AREA_STYLE('Steel - Satin',(#26150));
#26144=FILL_AREA_STYLE('CAD Library Painted - Graphite',(#26151));
#26145=FILL_AREA_STYLE('CAD Library Painted - Dark gray',(#26152));
#26146=FILL_AREA_STYLE('CAD Library Painted - Engineering blue',(#26153));
#26147=FILL_AREA_STYLE('CAD Library Painted - Steel gray',(#26154));
#26148=FILL_AREA_STYLE('CAD Library Painted - Light blue',(#26155));
#26149=FILL_AREA_STYLE('CAD Library Painted - Deep blue',(#26156));
#26150=FILL_AREA_STYLE_COLOUR('Steel - Satin',#26157);
#26151=FILL_AREA_STYLE_COLOUR('CAD Library Painted - Graphite',#26158);
#26152=FILL_AREA_STYLE_COLOUR('CAD Library Painted - Dark gray',#26159);
#26153=FILL_AREA_STYLE_COLOUR('CAD Library Painted - Engineering blue',
#26160);
#26154=FILL_AREA_STYLE_COLOUR('CAD Library Painted - Steel gray',#26161);
#26155=FILL_AREA_STYLE_COLOUR('CAD Library Painted - Light blue',#26162);
#26156=FILL_AREA_STYLE_COLOUR('CAD Library Painted - Deep blue',#26163);
#26157=COLOUR_RGB('Steel - Satin',0.627450980392157,0.627450980392157,0.627450980392157);
#26158=COLOUR_RGB('CAD Library Painted - Graphite',0.168627450980392,0.192156862745098,
0.231372549019608);
#26159=COLOUR_RGB('CAD Library Painted - Dark gray',0.325490196078431,0.364705882352941,
0.415686274509804);
#26160=COLOUR_RGB('CAD Library Painted - Engineering blue',0.12156862745098,
0.356862745098039,0.6);
#26161=COLOUR_RGB('CAD Library Painted - Steel gray',0.592156862745098,
0.631372549019608,0.67843137254902);
#26162=COLOUR_RGB('CAD Library Painted - Light blue',0.286274509803922,
0.552941176470588,0.780392156862745);
#26163=COLOUR_RGB('CAD Library Painted - Deep blue',0.0784313725490196,
0.203921568627451,0.349019607843137);
#26164=COLOUR_RGB('Dark Blue',0.08,0.2,0.34);
#26165=FILL_AREA_STYLE_COLOUR('',#26164);
#26166=FILL_AREA_STYLE('',(#26165));
#26167=SURFACE_STYLE_FILL_AREA(#26166);
#26168=SURFACE_SIDE_STYLE('',(#26167));
#26169=SURFACE_STYLE_USAGE(.BOTH.,#26168);
#26170=PRESENTATION_STYLE_ASSIGNMENT((#26169));
#26171=COLOUR_RGB('Light Blue',0.38,0.62,0.78);
#26172=FILL_AREA_STYLE_COLOUR('',#26171);
#26173=FILL_AREA_STYLE('',(#26172));
#26174=SURFACE_STYLE_FILL_AREA(#26173);
#26175=SURFACE_SIDE_STYLE('',(#26174));
#26176=SURFACE_STYLE_USAGE(.BOTH.,#26175);
#26177=PRESENTATION_STYLE_ASSIGNMENT((#26176));
#26178=COLOUR_RGB('Sky Blue',0.24,0.69,0.87);
#26179=FILL_AREA_STYLE_COLOUR('',#26178);
#26180=FILL_AREA_STYLE('',(#26179));
#26181=SURFACE_STYLE_FILL_AREA(#26180);
#26182=SURFACE_SIDE_STYLE('',(#26181));
#26183=SURFACE_STYLE_USAGE(.BOTH.,#26182);
#26184=PRESENTATION_STYLE_ASSIGNMENT((#26183));
#26185=COLOUR_RGB('Grey',0.48,0.52,0.57);
#26186=FILL_AREA_STYLE_COLOUR('',#26185);
#26187=FILL_AREA_STYLE('',(#26186));
#26188=SURFACE_STYLE_FILL_AREA(#26187);
#26189=SURFACE_SIDE_STYLE('',(#26188));
#26190=SURFACE_STYLE_USAGE(.BOTH.,#26189);
#26191=PRESENTATION_STYLE_ASSIGNMENT((#26190));
#26192=COLOUR_RGB('Black',0.12,0.14,0.17);
#26193=FILL_AREA_STYLE_COLOUR('',#26192);
#26194=FILL_AREA_STYLE('',(#26193));
#26195=SURFACE_STYLE_FILL_AREA(#26194);
#26196=SURFACE_SIDE_STYLE('',(#26195));
#26197=SURFACE_STYLE_USAGE(.BOTH.,#26196);
#26198=PRESENTATION_STYLE_ASSIGNMENT((#26197));
#26199=COLOUR_RGB('Off White',0.89,0.88,0.83);
#26200=FILL_AREA_STYLE_COLOUR('',#26199);
#26201=FILL_AREA_STYLE('',(#26200));
#26202=SURFACE_STYLE_FILL_AREA(#26201);
#26203=SURFACE_SIDE_STYLE('',(#26202));
#26204=SURFACE_STYLE_USAGE(.BOTH.,#26203);
#26205=PRESENTATION_STYLE_ASSIGNMENT((#26204));
ENDSEC;
END-ISO-10303-21;
